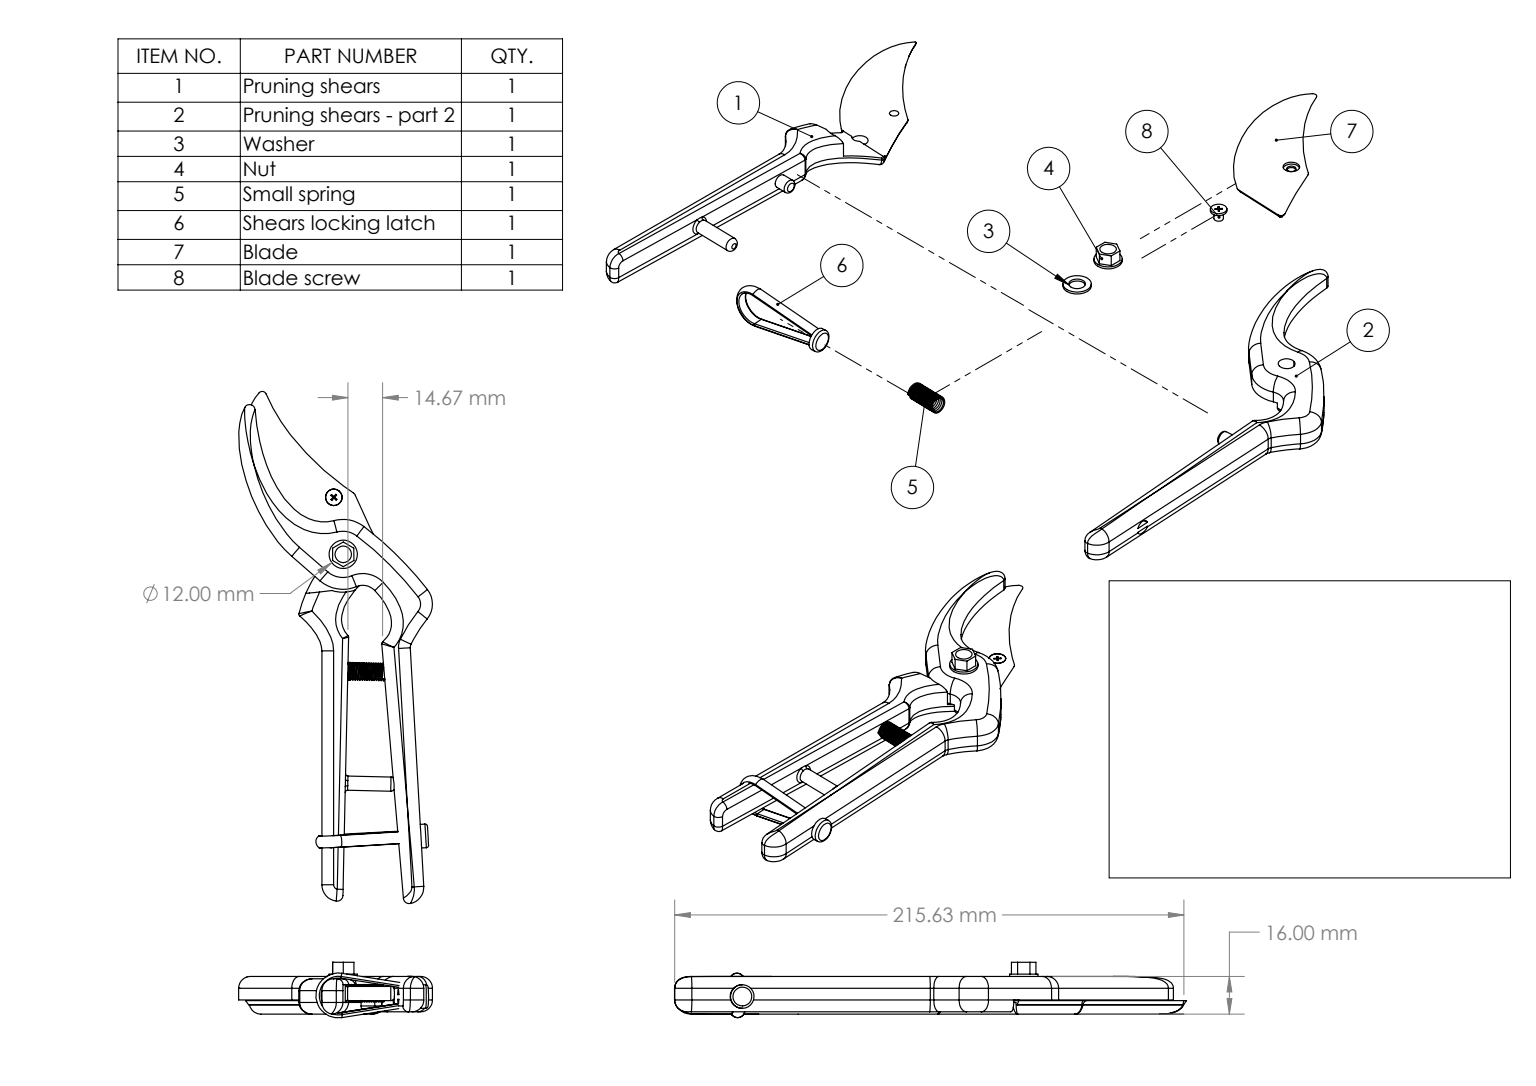
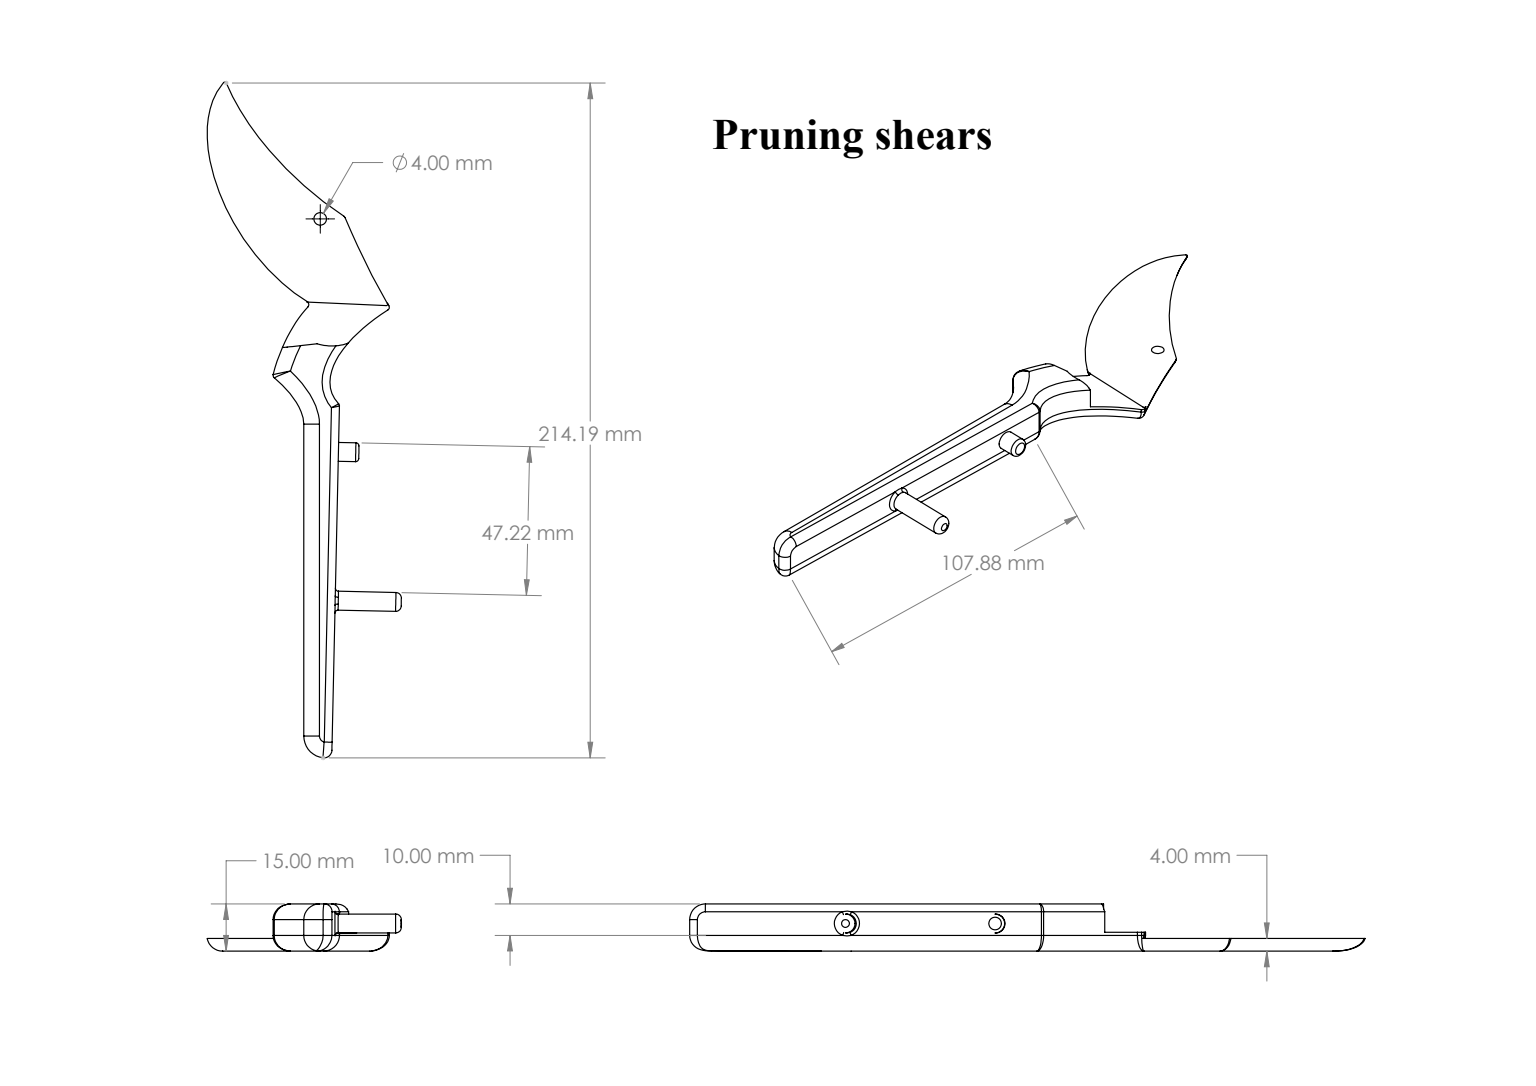
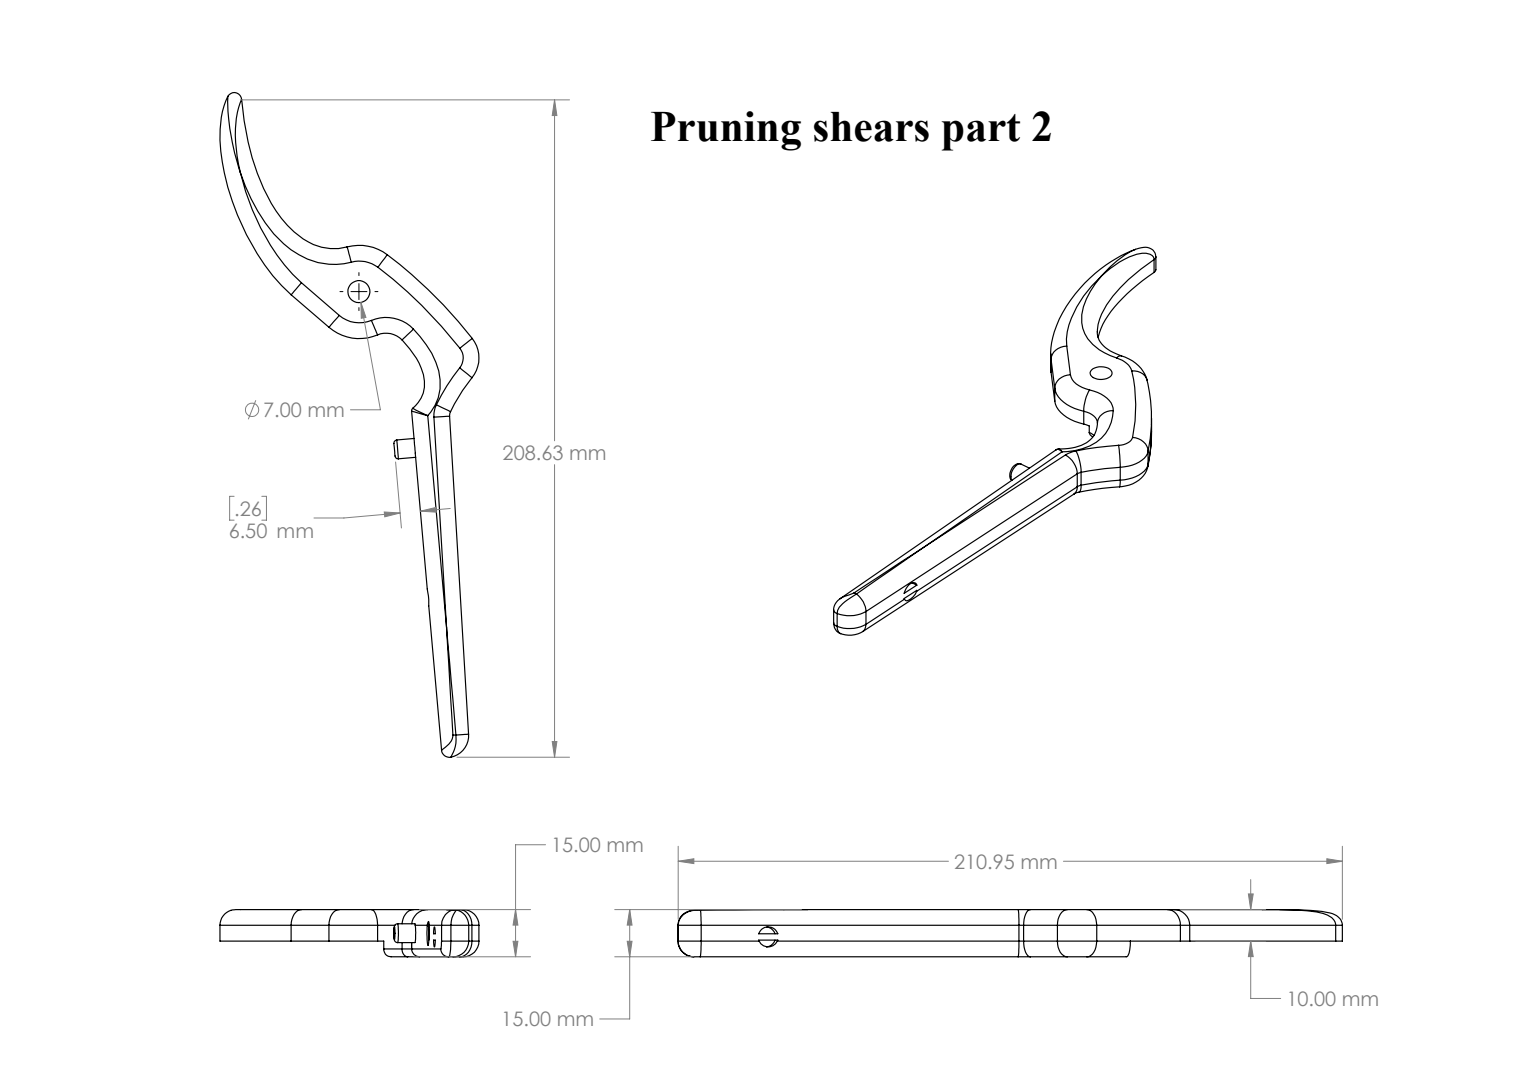
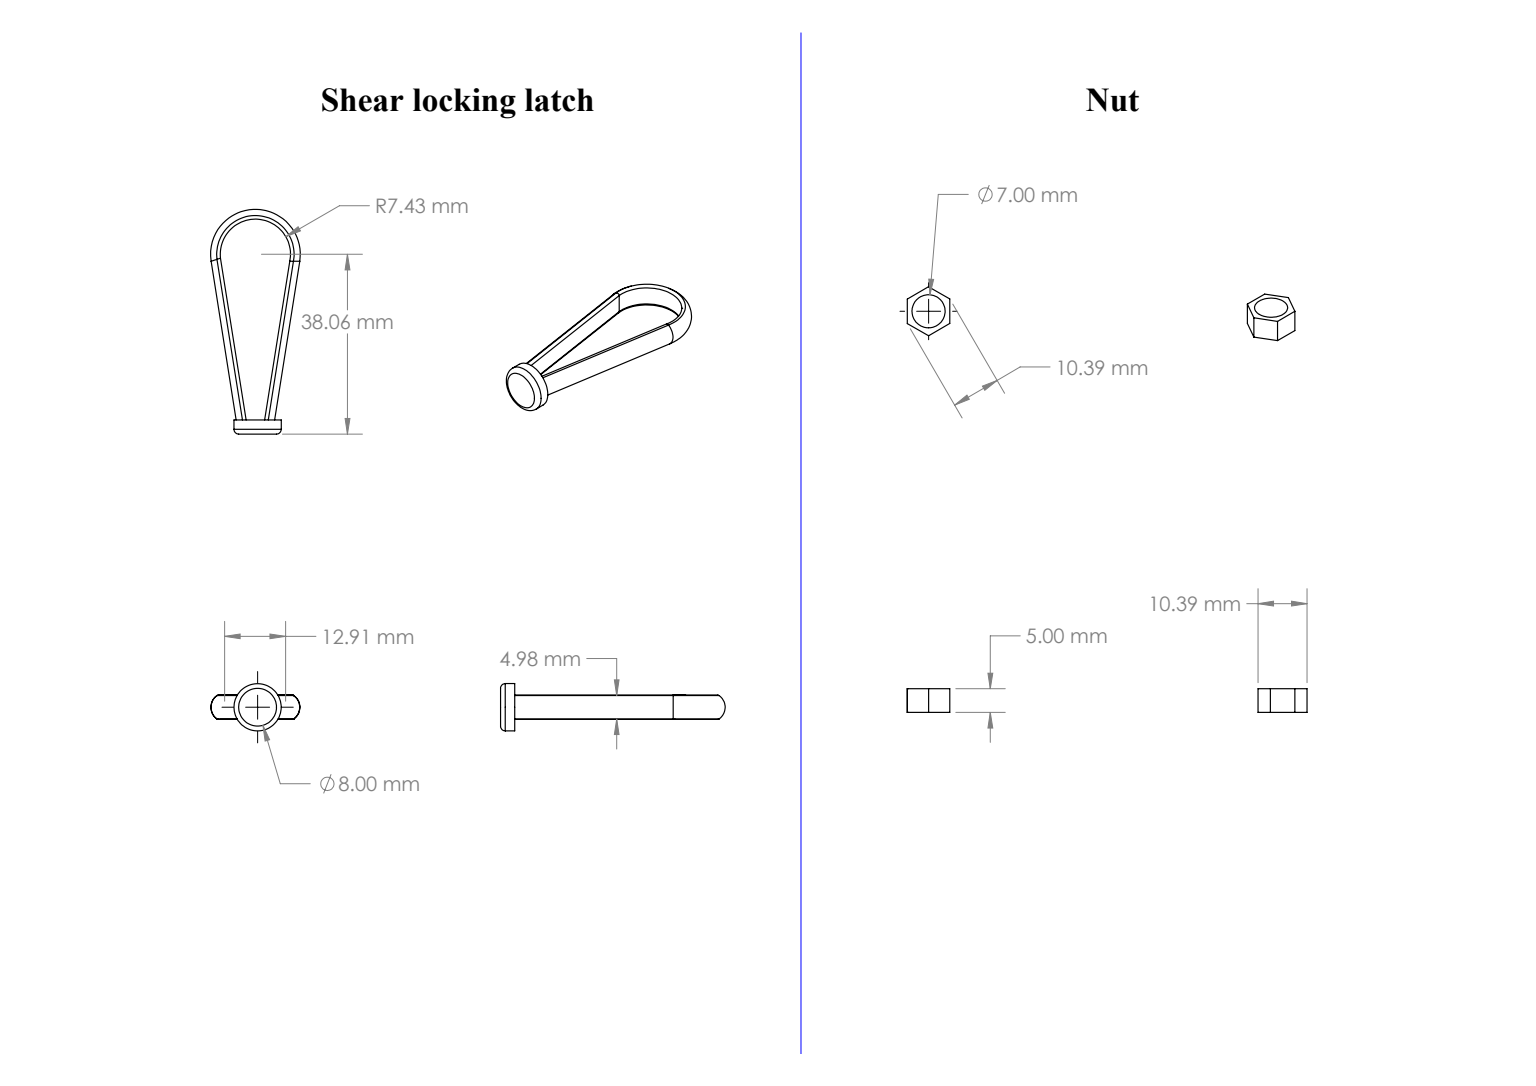
ISO-10303-21;
HEADER;
FILE_DESCRIPTION (('STEP AP203'),
    '1' );
FILE_NAME ('MAS-153',
    '2026-10-08T11:28:20',
    ( '' ),
    ( '' ),
    'SwSTEP 2.0',
    'SolidWorks 2024',
    '' );
FILE_SCHEMA (( 'AUTOMOTIVE_DESIGN' ));
ENDSEC;

DATA;
#1 = B_SPLINE_CURVE_WITH_KNOTS ( 'NONE', 3,
 ( #11082, #3985, #4982, #9929, #8605, #7599 ),
 .UNSPECIFIED., .F., .F.,
 ( 4, 2, 4 ),
 ( 0.000000000000000000, 0.0003771276215161150453, 0.0007542552430322300907 ),
 .UNSPECIFIED. ) ;
#2 = DIRECTION ( 'NONE',  ( 0.000000000000000000, 0.000000000000000000, -1.000000000000000000 ) ) ;
#3 = CARTESIAN_POINT ( 'NONE',  ( 3.749999999999999112, 3.187500000000000444, -5.053300858899108405 ) ) ;
#4 = DIRECTION ( 'NONE',  ( -0.9961255586397056438, 0.000000000000000000, 0.08794243244722428632 ) ) ;
#5 = CARTESIAN_POINT ( 'NONE',  ( -4.239466046644367658, 10.19338654090241114, -48.02051031032586081 ) ) ;
#6 = CARTESIAN_POINT ( 'NONE',  ( 8.895558325401111688, 6.000000000000000000, -141.4560052469132643 ) ) ;
#7 = CC_DESIGN_SECURITY_CLASSIFICATION ( #7654, ( #15322 ) ) ;
#8 = DIRECTION ( 'NONE',  ( 0.003262051938530752433, 0.000000000000000000, 0.9999946794944213346 ) ) ;
#9 = CARTESIAN_POINT ( 'NONE',  ( 3.249999999999999556, 12.75000000000000178, -3.500000000000000000 ) ) ;
#10 =( BOUNDED_SURFACE ( )  B_SPLINE_SURFACE ( 3, 2, ( 
 ( #2250, #5719, #10439 ),
 ( #12764, #3401, #13776 ),
 ( #9122, #8110, #5419 ),
 ( #12528, #2173, #793 ),
 ( #9278, #3171, #9054 ),
 ( #6877, #11445, #7884 ),
 ( #5641, #7962, #13852 ),
 ( #1011, #6953, #14952 ),
 ( #3250, #868, #2099 ),
 ( #10357, #4569, #1944 ),
 ( #15098, #11671, #12608 ),
 ( #4272, #6806, #14003 ),
 ( #12683, #8975, #11522 ),
 ( #3329, #938, #6657 ),
 ( #8038, #13706, #12837 ),
 ( #11370, #3105, #7816 ),
 ( #5571, #9201, #4347 ),
 ( #2023, #6733, #10286 ) ),
 .UNSPECIFIED., .F., .F., .F. ) 
 B_SPLINE_SURFACE_WITH_KNOTS ( ( 4, 2, 2, 2, 2, 2, 2, 2, 4 ),
 ( 3, 3 ),
 ( 0.06508395618386217385, 0.06791873945841907234, 0.07075352273297597083, 0.07217091437025441314, 0.07358830600753285545, 0.07642308928208975394, 0.07925787255664665243, 0.08209265583120353704, 0.08776222238031733403 ),
 ( 0.000000000000000000, 1.000000000000000000 ),
 .UNSPECIFIED. ) 
 GEOMETRIC_REPRESENTATION_ITEM ( )  RATIONAL_B_SPLINE_SURFACE ( (
 ( 1.000000000000000000, 0.7071067811865475727, 1.000000000000000000),
 ( 1.000000000000000000, 0.7071067811865475727, 1.000000000000000000),
 ( 1.000000000000000000, 0.7071067811865475727, 1.000000000000000000),
 ( 1.000000000000000000, 0.7071067811865475727, 1.000000000000000000),
 ( 1.000000000000000000, 0.7071067811865471286, 1.000000000000000000),
 ( 1.000000000000000000, 0.7071067811865471286, 1.000000000000000000),
 ( 1.000000000000000000, 0.7071067811865475727, 1.000000000000000000),
 ( 1.000000000000000000, 0.7071067811865475727, 1.000000000000000000),
 ( 1.000000000000000000, 0.7071067811865475727, 1.000000000000000000),
 ( 1.000000000000000000, 0.7071067811865475727, 1.000000000000000000),
 ( 1.000000000000000000, 0.7071067811865475727, 1.000000000000000000),
 ( 1.000000000000000000, 0.7071067811865475727, 1.000000000000000000),
 ( 1.000000000000000000, 0.7071067811865475727, 1.000000000000000000),
 ( 1.000000000000000000, 0.7071067811865475727, 1.000000000000000000),
 ( 1.000000000000000000, 0.7071067811865475727, 1.000000000000000000),
 ( 1.000000000000000000, 0.7071067811865475727, 1.000000000000000000),
 ( 1.000000000000000000, 0.7071067811865474617, 1.000000000000000000),
 ( 1.000000000000000000, 0.7071067811865474617, 1.000000000000000000) ) ) 
 REPRESENTATION_ITEM ( '' )  SURFACE ( )  );
#11 = AXIS2_PLACEMENT_3D ( 'NONE', #1949, #8982, #6882 ) ;
#12 = CARTESIAN_POINT ( 'NONE',  ( -25.82983890416511841, 9.999999999999998224, -142.4527639562402328 ) ) ;
#13 = CARTESIAN_POINT ( 'NONE',  ( -65.21690963830255328, 14.66435712545321657, -194.0246706955119009 ) ) ;
#14 = CIRCLE ( 'NONE', #8648, 3.500000000000003109 ) ;
#15 = ORIENTED_EDGE ( 'NONE', *, *, #9512, .T. ) ;
#16 = VERTEX_POINT ( 'NONE', #5138 ) ;
#17 = CARTESIAN_POINT ( 'NONE',  ( -6.279162092933343153, 2.500000000000000444, -108.6370948588273535 ) ) ;
#18 = CARTESIAN_POINT ( 'NONE',  ( 11.02991327057161008, 4.000000000000000000, -167.7534593579462125 ) ) ;
#19 = CARTESIAN_POINT ( 'NONE',  ( -3.750000000000000000, 6.250000000000000000, -3.499999999999999112 ) ) ;
#20 = CARTESIAN_POINT ( 'NONE',  ( 3.749999999999999556, 3.250000000000000000, -3.500000000000000444 ) ) ;
#21 = CARTESIAN_POINT ( 'NONE',  ( 1.114947364559086829, 5.000000000000000888, -139.4079432275550232 ) ) ;
#22 = ORIENTED_EDGE ( 'NONE', *, *, #13407, .T. ) ;
#23 = CARTESIAN_POINT ( 'NONE',  ( -6.510167201457561781, 0.4374612817596250647, -117.0692195733290504 ) ) ;
#24 = CARTESIAN_POINT ( 'NONE',  ( -2.298097038856279362, 0.8750000000000000000, -5.798097038856278473 ) ) ;
#25 = AXIS2_PLACEMENT_3D ( 'NONE', #11533, #14885, #11235 ) ;
#26 = CIRCLE ( 'NONE', #8661, 3.250000000000003553 ) ;
#27 = CARTESIAN_POINT ( 'NONE',  ( -46.17421409260412446, 15.00000000000000000, -147.1483150044805939 ) ) ;
#28 = CIRCLE ( 'NONE', #12604, 8.192786906463668473 ) ;
#29 = CARTESIAN_POINT ( 'NONE',  ( 14.17870013830592235, 8.673617379884035472E-16, -133.6038822290509813 ) ) ;
#30 = DIRECTION ( 'NONE',  ( 1.000000000000000000, 0.000000000000000000, 0.000000000000000000 ) ) ;
#31 = CARTESIAN_POINT ( 'NONE',  ( 0.000000000000000000, 3.000000000000000000, -0.2500000000000002220 ) ) ;
#32 = COORDINATED_UNIVERSAL_TIME_OFFSET ( 0, 0, .AHEAD. ) ;
#33 = CARTESIAN_POINT ( 'NONE',  ( 17.45707370880436216, 8.749999999999998224, -89.70141063960701899 ) ) ;
#34 = CARTESIAN_POINT ( 'NONE',  ( 12.21230042249527514, -8.519112334771948619E-13, -124.0782217032746217 ) ) ;
#35 = ORIENTED_EDGE ( 'NONE', *, *, #13499, .F. ) ;
#36 = CARTESIAN_POINT ( 'NONE',  ( -8.661991262811106651, 15.00000000000000000, -130.6821289911104316 ) ) ;
#37 = CARTESIAN_POINT ( 'NONE',  ( -3.249999999999999556, 14.18750000000000000, -2.153805922287440833 ) ) ;
#38 = AXIS2_PLACEMENT_3D ( 'NONE', #940, #8979, #1799 ) ;
#39 = ORIENTED_EDGE ( 'NONE', *, *, #8561, .F. ) ;
#40 = VERTEX_POINT ( 'NONE', #4981 ) ;
#41 = DIRECTION ( 'NONE',  ( -0.000000000000000000, -1.000000000000000000, -0.000000000000000000 ) ) ;
#42 = CARTESIAN_POINT ( 'NONE',  ( 1.553300858899105963, 4.062500000000001776, -7.250000000000000888 ) ) ;
#43 = CARTESIAN_POINT ( 'NONE',  ( -1.346194077712559167, 5.937500000000002665, -6.749999999999999112 ) ) ;
#44 = ORIENTED_EDGE ( 'NONE', *, *, #4143, .F. ) ;
#45 = EDGE_CURVE ( 'NONE', #5739, #9776, #9697, .T. ) ;
#46 = CARTESIAN_POINT ( 'NONE',  ( 4.515869450399739193, 15.00000000000000000, -104.3391973869742060 ) ) ;
#47 = CARTESIAN_POINT ( 'NONE',  ( 1.346194077712558057, 4.562500000000000888, -6.750000000000000000 ) ) ;
#48 = VECTOR ( 'NONE', #1448, 1000.000000000000114 ) ;
#49 = DIRECTION ( 'NONE',  ( -0.002879925520664897674, 0.000000000000000000, -0.9999958530058988826 ) ) ;
#50 = DIRECTION ( 'NONE',  ( 0.000000000000000000, 0.000000000000000000, 1.000000000000000000 ) ) ;
#51 = CARTESIAN_POINT ( 'NONE',  ( -9.030574454602202650, -2.490287375297125294, -34.97919997656153157 ) ) ;
#52 = PERSON_AND_ORGANIZATION ( #3176, #3020 ) ;
#53 = CARTESIAN_POINT ( 'NONE',  ( -48.96897228669091362, 15.00000000000000178, -150.1829960677724500 ) ) ;
#54 = ORIENTED_EDGE ( 'NONE', *, *, #7438, .F. ) ;
#55 =( GEOMETRIC_REPRESENTATION_CONTEXT ( 3 ) GLOBAL_UNCERTAINTY_ASSIGNED_CONTEXT ( ( #2945 ) ) GLOBAL_UNIT_ASSIGNED_CONTEXT ( ( #13919, #7590, #5627 ) ) REPRESENTATION_CONTEXT ( 'NONE', 'WORKASPACE' ) );
#56 = EDGE_CURVE ( 'NONE', #9845, #1534, #14253, .T. ) ;
#57 = DIRECTION ( 'NONE',  ( 0.08794243244723005948, 0.000000000000000000, 0.9961255586397049777 ) ) ;
#58 = ADVANCED_FACE ( 'NONE', ( #12392 ), #3118, .T. ) ;
#59 = CARTESIAN_POINT ( 'NONE',  ( 2.651650429449553314, 14.37500000000000000, -0.8483495705504476847 ) ) ;
#60 = FACE_OUTER_BOUND ( 'NONE', #10831, .T. ) ;
#61 = CARTESIAN_POINT ( 'NONE',  ( -67.60837051205176351, 11.42435839016798838, -204.0214325388246266 ) ) ;
#62 = CARTESIAN_POINT ( 'NONE',  ( 0.5457951471881908878, 3.606183382230925272, -138.3638248956704047 ) ) ;
#63 = CARTESIAN_POINT ( 'NONE',  ( -3.249999999999999556, 3.750000000000000444, -3.500000000000000000 ) ) ;
#64 = CARTESIAN_POINT ( 'NONE',  ( 9.455311519598982528, 14.93740492236557138, -106.0041704794325454 ) ) ;
#65 = APPROVAL_STATUS ( 'not_yet_approved' ) ;
#66 = CARTESIAN_POINT ( 'NONE',  ( -29.69515346086419427, 5.000000000000000888, -156.7390981038714983 ) ) ;
#67 = CARTESIAN_POINT ( 'NONE',  ( -17.09940774937029317, 0.4261086865563343262, -130.4730999849509203 ) ) ;
#68 = ORIENTED_EDGE ( 'NONE', *, *, #7323, .F. ) ;
#69 = CARTESIAN_POINT ( 'NONE',  ( 5.522929128040925839, 0.1436561706274334937, 1.641076506811401270 ) ) ;
#70 = CARTESIAN_POINT ( 'NONE',  ( -3.249999999999999556, 1.250000000000000000, -3.499999999999999556 ) ) ;
#71 = AXIS2_PLACEMENT_3D ( 'NONE', #14775, #7400, #12125 ) ;
#72 = CARTESIAN_POINT ( 'NONE',  ( -63.46632602869123474, 15.00000000000000000, -179.6775508400713477 ) ) ;
#73 = CARTESIAN_POINT ( 'NONE',  ( 2.298097038856278029, 7.125000000000000888, -5.798097038856279362 ) ) ;
#74 = ORIENTED_EDGE ( 'NONE', *, *, #3541, .T. ) ;
#75 = CARTESIAN_POINT ( 'NONE',  ( -5.117107008692297399, 9.999999999999998224, -113.5915292474705893 ) ) ;
#76 = EDGE_CURVE ( 'NONE', #2801, #15277, #3494, .T. ) ;
#77 = CARTESIAN_POINT ( 'NONE',  ( 21.59580923397518859, 6.000000000000000000, -133.6052420832058374 ) ) ;
#78 = CARTESIAN_POINT ( 'NONE',  ( 9.096999351293019842, 14.99999999999896438, -106.0212576677412812 ) ) ;
#79 = CARTESIAN_POINT ( 'NONE',  ( 2.298097038856279362, 1.875000000000000000, -1.201902961143720860 ) ) ;
#80 = CARTESIAN_POINT ( 'NONE',  ( -1.553300858899107073, 1.937500000000000222, -7.249999999999999112 ) ) ;
#81 = APPLICATION_CONTEXT ( 'configuration controlled 3d designs of mechanical parts and assemblies' ) ;
#82 = CARTESIAN_POINT ( 'NONE',  ( -3.750000000000000000, 7.312500000000000000, -5.053300858899105741 ) ) ;
#83 = CARTESIAN_POINT ( 'NONE',  ( -0.2962205294200081496, 8.673617379884033500E-16, -113.2751335308100096 ) ) ;
#84 = CARTESIAN_POINT ( 'NONE',  ( 3.749999999999999556, 4.250000000000000000, -3.500000000000000444 ) ) ;
#85 = CIRCLE ( 'NONE', #9462, 0.4999999999999865663 ) ;
#86 = CARTESIAN_POINT ( 'NONE',  ( 1.062740323768540662, 12.59030360039310636, 5.094619354848065385 ) ) ;
#87 = DIRECTION ( 'NONE',  ( 0.000000000000000000, 0.000000000000000000, -1.000000000000000000 ) ) ;
#88 = CARTESIAN_POINT ( 'NONE',  ( -0.3675725891509493137, 0.000000000000000000, -0.3389548520155291622 ) ) ;
#89 = LINE ( 'NONE', #4800, #3326 ) ;
#90 = CARTESIAN_POINT ( 'NONE',  ( 1.346194077712560944, 10.93750000000000000, -0.2500000000000010547 ) ) ;
#91 = CARTESIAN_POINT ( 'NONE',  ( 8.807773658247754156, 15.00000000000000000, -105.8689255569352667 ) ) ;
#92 = CARTESIAN_POINT ( 'NONE',  ( -63.21422130130005712, 10.26968228116884596, -203.6040552426024988 ) ) ;
#93 = ORIENTED_EDGE ( 'NONE', *, *, #14365, .F. ) ;
#94 = ORIENTED_EDGE ( 'NONE', *, *, #15196, .T. ) ;
#95 = CARTESIAN_POINT ( 'NONE',  ( -4.723546506723169003, 4.336808689942017736E-16, -121.1708306026675501 ) ) ;
#96 = CARTESIAN_POINT ( 'NONE',  ( 10.93680211553660619, 8.749999999999998224, -88.84347220940026091 ) ) ;
#97 = CARTESIAN_POINT ( 'NONE',  ( 3.749999999999998668, 4.687500000000000888, -5.053300858899107517 ) ) ;
#98 = AXIS2_PLACEMENT_3D ( 'NONE', #12343, #1762, #3856 ) ;
#99 = CARTESIAN_POINT ( 'NONE',  ( -3.750000000000000000, 5.812500000000000888, -5.053300858899105741 ) ) ;
#100 = AXIS2_PLACEMENT_3D ( 'NONE', #7008, #14909, #675 ) ;
#101 = DIRECTION ( 'NONE',  ( -0.02181900108494732801, 0.000000000000000000, 0.9997619372588931741 ) ) ;
#102 = ORIENTED_EDGE ( 'NONE', *, *, #10097, .F. ) ;
#103 = CARTESIAN_POINT ( 'NONE',  ( 3.249999999999998224, 3.187500000000000444, -4.846194077712561388 ) ) ;
#104 = CARTESIAN_POINT ( 'NONE',  ( -54.45540687895485377, 9.999999999999998224, -149.0501727870129685 ) ) ;
#105 = DIRECTION ( 'NONE',  ( 0.000000000000000000, 1.000000000000000000, 0.000000000000000000 ) ) ;
#106 = CARTESIAN_POINT ( 'NONE',  ( -2.298097038856278918, 2.375000000000000000, -5.798097038856277585 ) ) ;
#107 = AXIS2_PLACEMENT_3D ( 'NONE', #15128, #4596, #14185 ) ;
#108 = PERSON_AND_ORGANIZATION_ROLE ( 'classification_officer' ) ;
#109 = CARTESIAN_POINT ( 'NONE',  ( 10.14688567188825274, 12.49999999999999822, -108.1982192590441088 ) ) ;
#110 = CARTESIAN_POINT ( 'NONE',  ( 16.81337476685454391, 5.000000000000000888, -129.2521154345601246 ) ) ;
#111 = ORIENTED_EDGE ( 'NONE', *, *, #10885, .F. ) ;
#112 = CARTESIAN_POINT ( 'NONE',  ( -0.5447792503669787179, 14.99999999999999467, -117.0548960884185732 ) ) ;
#113 = CARTESIAN_POINT ( 'NONE',  ( 1.346194077712560944, 14.93750000000000178, -0.2500000000000011102 ) ) ;
#114 = VERTEX_POINT ( 'NONE', #6524 ) ;
#115 = EDGE_LOOP ( 'NONE', ( #2577, #6448, #3644, #14462 ) ) ;
#116 = DIRECTION ( 'NONE',  ( -0.000000000000000000, -1.000000000000000000, -0.000000000000000000 ) ) ;
#117 = CARTESIAN_POINT ( 'NONE',  ( -4.592425496802573972E-16, 5.000000000000000000, -7.250000000000000000 ) ) ;
#118 = CARTESIAN_POINT ( 'NONE',  ( -1.346194077712558945, 10.56249999999999822, -0.2500000000000002220 ) ) ;
#119 = VERTEX_POINT ( 'NONE', #1731 ) ;
#120 = CARTESIAN_POINT ( 'NONE',  ( -1.334601435215557519, 9.999999999999998224, -105.6792246796216403 ) ) ;
#121 = CIRCLE ( 'NONE', #7519, 4.999999999999995559 ) ;
#122 = CARTESIAN_POINT ( 'NONE',  ( 1.346194077712558057, 3.562500000000000444, -6.750000000000000000 ) ) ;
#123 = CARTESIAN_POINT ( 'NONE',  ( -7.332173456847238313, 0.07668794466513038921, -104.2603615701598869 ) ) ;
#124 = CARTESIAN_POINT ( 'NONE',  ( -62.71861979978048396, 10.00000000000000000, -198.6004802465432135 ) ) ;
#125 = AXIS2_PLACEMENT_3D ( 'NONE', #9268, #6866, #11579 ) ;
#126 = SHAPE_DEFINITION_REPRESENTATION ( #5707, #10790 ) ;
#127 = CARTESIAN_POINT ( 'NONE',  ( -52.99646050385619844, 15.00000000000000000, -155.6021463114098253 ) ) ;
#128 = ORIENTED_EDGE ( 'NONE', *, *, #6104, .F. ) ;
#129 = CARTESIAN_POINT ( 'NONE',  ( -3.249999999999999556, 9.187500000000000000, -2.153805922287440833 ) ) ;
#130 = CARTESIAN_POINT ( 'NONE',  ( -4.234402844927150689, 15.00000000000000000, -117.4888040839639558 ) ) ;
#131 = CARTESIAN_POINT ( 'NONE',  ( -4.592425496802573972E-16, 14.00000000000000000, -7.250000000000000000 ) ) ;
#132 = CARTESIAN_POINT ( 'NONE',  ( 0.000000000000000000, 0.000000000000000000, -2.000000000000000000 ) ) ;
#133 = B_SPLINE_CURVE_WITH_KNOTS ( 'NONE', 3,
 ( #5793, #4490, #6875, #8036, #2247, #9119, #866, #3327, #10513, #12761, #13773, #3478, #11520, #10215, #15248, #4639, #8187, #5717, #11590, #14950, #12912, #2325, #9052, #7024 ),
 .UNSPECIFIED., .F., .F.,
 ( 4, 2, 2, 2, 2, 2, 2, 2, 2, 2, 2, 4 ),
 ( 0.001027084968682773474, 0.001754664737541044694, 0.002482244506399315480, 0.003937404044115912563, 0.004664983812974211538, 0.005392563581832510514, 0.006847723119549108464, 0.009758042194982304365, 0.01121320173269890232, 0.01194078150155724292, 0.01230457138598641496, 0.01266836127041558527 ),
 .UNSPECIFIED. ) ;
#134 = CARTESIAN_POINT ( 'NONE',  ( -63.23239576043733479, 10.46432717375524213, -203.5646039687676705 ) ) ;
#135 = CARTESIAN_POINT ( 'NONE',  ( 0.5065669489467078401, 5.000000000003537615, 5.737893198614711032 ) ) ;
#136 = CARTESIAN_POINT ( 'NONE',  ( 1.346194077712561166, 4.437500000000001776, -0.2500000000000011102 ) ) ;
#137 = ADVANCED_FACE ( 'NONE', ( #11160 ), #2010, .F. ) ;
#138 = CARTESIAN_POINT ( 'NONE',  ( 9.910078351765200466, 14.75237657882121667, -106.1010689402279468 ) ) ;
#139 = PERSON_AND_ORGANIZATION ( #3176, #3020 ) ;
#140 = EDGE_CURVE ( 'NONE', #13676, #587, #14399, .T. ) ;
#141 = CARTESIAN_POINT ( 'NONE',  ( 1.855481649321436777, 15.00000000000000000, -35.83830032691820122 ) ) ;
#142 = CARTESIAN_POINT ( 'NONE',  ( 0.000000000000000000, 5.000000000000000000, -3.500000000000000000 ) ) ;
#143 = EDGE_LOOP ( 'NONE', ( #10004, #6723, #11790, #8217 ) ) ;
#144 = CARTESIAN_POINT ( 'NONE',  ( 5.475582110871519248, 2.099780042704602945, 4.221432182364227792 ) ) ;
#145 = CARTESIAN_POINT ( 'NONE',  ( 2.298097038856279362, 1.875000000000000000, -1.201902961143720860 ) ) ;
#146 = CARTESIAN_POINT ( 'NONE',  ( -9.240119717473294969, 2.324218168632100845, -104.6630069163585972 ) ) ;
#147 = CARTESIAN_POINT ( 'NONE',  ( 3.249999999999999556, 14.75000000000000178, -3.500000000000000000 ) ) ;
#148 = CARTESIAN_POINT ( 'NONE',  ( -1.346194077712559167, 5.937500000000002665, -6.749999999999999112 ) ) ;
#149 = ORIENTED_EDGE ( 'NONE', *, *, #4890, .T. ) ;
#150 = CARTESIAN_POINT ( 'NONE',  ( -5.893421222731322295, 9.999999999999998224, -117.5694263798337005 ) ) ;
#151 = DIRECTION ( 'NONE',  ( 0.000000000000000000, 1.000000000000000000, 0.000000000000000000 ) ) ;
#152 = CARTESIAN_POINT ( 'NONE',  ( 1.818681402055029483, 15.00000000000000000, -137.3269588978979243 ) ) ;
#153 = CC_DESIGN_DATE_AND_TIME_ASSIGNMENT ( #8465, #10947, ( #9370 ) ) ;
#154 = CARTESIAN_POINT ( 'NONE',  ( -2.298097038856278918, 0.3750000000000000000, -5.798097038856277585 ) ) ;
#155 = CARTESIAN_POINT ( 'NONE',  ( 2.651650429449552870, 1.124999999999999778, -6.151650429449553314 ) ) ;
#156 = CARTESIAN_POINT ( 'NONE',  ( -2.651650429449552870, 4.125000000000000000, -0.8483495705504462414 ) ) ;
#157 = CARTESIAN_POINT ( 'NONE',  ( -5.309262520577839872, 13.36526483154179523, -125.0911079416483176 ) ) ;
#158 = CARTESIAN_POINT ( 'NONE',  ( 2.651650429449552870, 8.125000000000000000, -6.151650429449555091 ) ) ;
#159 = CARTESIAN_POINT ( 'NONE',  ( 0.9143209798285035772, 12.53633980243307100, 2.514521240264253166 ) ) ;
#160 = DIRECTION ( 'NONE',  ( 0.000000000000000000, -0.000000000000000000, 1.000000000000000000 ) ) ;
#161 = EDGE_CURVE ( 'NONE', #6131, #12717, #6840, .T. ) ;
#162 = EDGE_CURVE ( 'NONE', #10108, #12142, #11036, .T. ) ;
#163 = DIRECTION ( 'NONE',  ( -0.000000000000000000, 1.000000000000000000, -0.000000000000000000 ) ) ;
#164 = EDGE_CURVE ( 'NONE', #10316, #6640, #6443, .T. ) ;
#165 = FACE_OUTER_BOUND ( 'NONE', #967, .T. ) ;
#166 = CARTESIAN_POINT ( 'NONE',  ( 0.000000000000000000, 14.00000000000000000, -0.2500000000000002220 ) ) ;
#167 = CARTESIAN_POINT ( 'NONE',  ( 8.617011912565523346, 3.196949058014985745, 2.666643044219553893 ) ) ;
#168 = CARTESIAN_POINT ( 'NONE',  ( -64.38825976928389139, 13.56900998018364213, -200.2675612624753398 ) ) ;
#169 = ORIENTED_EDGE ( 'NONE', *, *, #3673, .F. ) ;
#170 = CARTESIAN_POINT ( 'NONE',  ( -3.749999999999999556, 8.750000000000000000, -3.499999999999999112 ) ) ;
#171 = EDGE_LOOP ( 'NONE', ( #12222, #10076, #8001, #12391 ) ) ;
#172 = CARTESIAN_POINT ( 'NONE',  ( -6.790118584858316986, 2.500000000000000444, -107.8021323224912464 ) ) ;
#173 = CARTESIAN_POINT ( 'NONE',  ( -10.72138378296756756, -1.921202954650397476, -40.62330995231929620 ) ) ;
#174 = CARTESIAN_POINT ( 'NONE',  ( 1.553300858899108849, 9.937499999999998224, 0.2499999999999993616 ) ) ;
#175 = CARTESIAN_POINT ( 'NONE',  ( -3.749999999999999556, 5.750000000000000000, -3.499999999999999112 ) ) ;
#176 = DIRECTION ( 'NONE',  ( -0.9997619372588932851, -0.000000000000000000, -0.02181900108494707474 ) ) ;
#177 = ORIENTED_EDGE ( 'NONE', *, *, #10342, .F. ) ;
#178 = CARTESIAN_POINT ( 'NONE',  ( -2.298097038856278029, 2.625000000000000000, -1.201902961143720638 ) ) ;
#179 = CARTESIAN_POINT ( 'NONE',  ( -69.61556017177876754, 9.999999999999998224, -198.3353672694111083 ) ) ;
#180 = CARTESIAN_POINT ( 'NONE',  ( 19.46764420669212470, 5.416677968589100837E-32, -137.9817351395554681 ) ) ;
#181 = CARTESIAN_POINT ( 'NONE',  ( 2.298097038856279362, 6.875000000000000000, -1.201902961143720860 ) ) ;
#182 = CARTESIAN_POINT ( 'NONE',  ( -1.794496370643203553, 15.00000000000000711, -123.9659188807642920 ) ) ;
#183 = APPROVAL_ROLE ( '' ) ;
#184 = CARTESIAN_POINT ( 'NONE',  ( -4.891470111510197505, 6.071532165918824830E-15, -115.0631877436127581 ) ) ;
#185 = CARTESIAN_POINT ( 'NONE',  ( 20.93263444585494781, -4.267469463954428261E-13, -132.7914611339567159 ) ) ;
#186 = CC_DESIGN_DATE_AND_TIME_ASSIGNMENT ( #10259, #7786, ( #13819 ) ) ;
#187 = ORIENTED_EDGE ( 'NONE', *, *, #1290, .T. ) ;
#188 = CARTESIAN_POINT ( 'NONE',  ( -1.260792021077014269, 15.00000000000000178, -107.5178971017766258 ) ) ;
#189 = CARTESIAN_POINT ( 'NONE',  ( -3.980102097228897245E-16, 14.50000000000000000, -6.749999999999999112 ) ) ;
#190 = ORIENTED_EDGE ( 'NONE', *, *, #14252, .F. ) ;
#191 = VERTEX_POINT ( 'NONE', #10233 ) ;
#192 = CARTESIAN_POINT ( 'NONE',  ( 22.32840821305085655, 0.1344125794277489794, -138.8040290914306922 ) ) ;
#193 = CARTESIAN_POINT ( 'NONE',  ( 2.651650429449552870, 7.125000000000000888, -6.151650429449555091 ) ) ;
#194 = CARTESIAN_POINT ( 'NONE',  ( -2.298097038856279362, 8.874999999999996447, -5.798097038856278473 ) ) ;
#195 = ORIENTED_EDGE ( 'NONE', *, *, #5701, .F. ) ;
#196 = CARTESIAN_POINT ( 'NONE',  ( 6.130233522805849766, 11.30590447954031497, 5.118507051967887911 ) ) ;
#197 = CARTESIAN_POINT ( 'NONE',  ( -3.249999999999999556, 5.187500000000001776, -2.153805922287440833 ) ) ;
#198 = CARTESIAN_POINT ( 'NONE',  ( -9.222297982611349809, 2.161611222164042001, -104.6591137165734864 ) ) ;
#199 = CARTESIAN_POINT ( 'NONE',  ( -33.91109452337774854, 10.00000000000000178, -156.1716796081737471 ) ) ;
#200 = CARTESIAN_POINT ( 'NONE',  ( -45.43402158771803556, 15.00000000000000355, -154.4665057826428267 ) ) ;
#201 = APPROVAL_ROLE ( '' ) ;
#202 = CARTESIAN_POINT ( 'NONE',  ( -62.77354874813351415, 14.99999999999999822, -176.9788886477732035 ) ) ;
#203 = ORIENTED_EDGE ( 'NONE', *, *, #9865, .F. ) ;
#204 = CARTESIAN_POINT ( 'NONE',  ( -3.249999999999999556, 0.3125000000000000555, -4.846194077712557835 ) ) ;
#205 = CARTESIAN_POINT ( 'NONE',  ( -0.9850606648477213678, 15.00000000000000000, -125.5681744140592144 ) ) ;
#206 = CARTESIAN_POINT ( 'NONE',  ( -3.750000000000000000, 12.81250000000000178, -5.053300858899105741 ) ) ;
#207 = CARTESIAN_POINT ( 'NONE',  ( -67.63619164393119831, 12.59430211938552802, -202.7040278164101323 ) ) ;
#208 = DIRECTION ( 'NONE',  ( -0.9997619372588932851, -0.000000000000000000, -0.02181900108494707821 ) ) ;
#209 = CARTESIAN_POINT ( 'NONE',  ( 1.346194077712561166, 3.437500000000000444, -0.2500000000000011102 ) ) ;
#210 = CARTESIAN_POINT ( 'NONE',  ( 9.985685122837379524, 1.585996910455645059, -106.2985558885148833 ) ) ;
#211 = PERSON_AND_ORGANIZATION ( #3176, #3020 ) ;
#212 = CARTESIAN_POINT ( 'NONE',  ( -2.555845825458327170, 14.83119756125146438, -125.3948779398220381 ) ) ;
#213 = CARTESIAN_POINT ( 'NONE',  ( -9.030574454602195544, -2.490287375297125294, -34.97919997656152447 ) ) ;
#214 = ORIENTED_EDGE ( 'NONE', *, *, #4803, .T. ) ;
#215 = CARTESIAN_POINT ( 'NONE',  ( 5.309569511722092905, 0.1704923354856621165, -0.3824473862144103231 ) ) ;
#216 = CARTESIAN_POINT ( 'NONE',  ( -2.298097038856278918, 8.375000000000000000, -5.798097038856277585 ) ) ;
#217 = CARTESIAN_POINT ( 'NONE',  ( -63.86794096056340209, 10.00000000000000000, -165.1728739221729825 ) ) ;
#218 = CARTESIAN_POINT ( 'NONE',  ( 2.298097038856278473, 14.62500000000000000, -5.798097038856279362 ) ) ;
#219 = EDGE_CURVE ( 'NONE', #9239, #1748, #2967, .T. ) ;
#220 = CARTESIAN_POINT ( 'NONE',  ( 0.000000000000000000, 7.500000000000000888, -0.2500000000000002220 ) ) ;
#221 = CARTESIAN_POINT ( 'NONE',  ( -0.5758322980023804494, 15.00000000000000000, -117.2003571699043221 ) ) ;
#222 = DIRECTION ( 'NONE',  ( 0.000000000000000000, 0.000000000000000000, 1.000000000000000000 ) ) ;
#223 = CARTESIAN_POINT ( 'NONE',  ( 6.020998550613693823, 15.00000000000000000, -132.6181299100952629 ) ) ;
#224 = EDGE_CURVE ( 'NONE', #10778, #11957, #683, .T. ) ;
#225 = CARTESIAN_POINT ( 'NONE',  ( 2.298097038856278473, 1.625000000000000222, -5.798097038856279362 ) ) ;
#226 = CARTESIAN_POINT ( 'NONE',  ( -2.651650429449552870, 2.625000000000000000, -0.8483495705504467965 ) ) ;
#227 = CARTESIAN_POINT ( 'NONE',  ( 1.553300858899108849, 4.937500000000000888, 0.2499999999999993616 ) ) ;
#228 = CARTESIAN_POINT ( 'NONE',  ( -4.160651409637847742, 10.31235003438523989, -46.92824181062579214 ) ) ;
#229 = CARTESIAN_POINT ( 'NONE',  ( 1.553300858899105963, 6.062500000000000888, -7.250000000000000888 ) ) ;
#230 = CARTESIAN_POINT ( 'NONE',  ( 1.674841001514616012, 13.54983687837186146, 4.356007712918980701 ) ) ;
#231 = CARTESIAN_POINT ( 'NONE',  ( -3.806000526524415672, 10.67725751578602633, -43.60682525637299989 ) ) ;
#232 =( BOUNDED_SURFACE ( )  B_SPLINE_SURFACE ( 3, 1, ( 
 ( #3931, #529 ),
 ( #12031, #14691 ),
 ( #8632, #9877 ),
 ( #298, #8796 ) ),
 .UNSPECIFIED., .F., .F., .T. ) 
 B_SPLINE_SURFACE_WITH_KNOTS ( ( 4, 4 ),
 ( 2, 2 ),
 ( 0.000000000000000000, 1.000000000000000000 ),
 ( 0.000000000000000000, 1.000000000000000000 ),
 .UNSPECIFIED. ) 
 GEOMETRIC_REPRESENTATION_ITEM ( )  RATIONAL_B_SPLINE_SURFACE ( (
 ( 1.000000000000000000, 1.000000000000000000),
 ( 0.6468719831415908894, 0.6468719831415908894),
 ( 0.6468719831415908894, 0.6468719831415908894),
 ( 1.000000000000000000, 1.000000000000000000) ) ) 
 REPRESENTATION_ITEM ( '' )  SURFACE ( )  );
#233 = FACE_OUTER_BOUND ( 'NONE', #599, .T. ) ;
#234 = CC_DESIGN_DATE_AND_TIME_ASSIGNMENT ( #2614, #2772, ( #2984 ) ) ;
#235 = DIRECTION ( 'NONE',  ( 0.9997619372588932851, -0.000000000000000000, 0.02181900108494707474 ) ) ;
#236 = LINE ( 'NONE', #6346, #3220 ) ;
#237 = CARTESIAN_POINT ( 'NONE',  ( -19.59630400042128784, 8.673617379884035472E-16, -169.8472985358678216 ) ) ;
#238 = CARTESIAN_POINT ( 'NONE',  ( 9.939878312292623974, 5.000000000000000888, -115.2320631035898373 ) ) ;
#239 = CARTESIAN_POINT ( 'NONE',  ( 1.346194077712560944, 8.937500000000001776, -0.2500000000000010547 ) ) ;
#240 = ORIENTED_EDGE ( 'NONE', *, *, #10815, .T. ) ;
#241 = LOCAL_TIME ( 12, 28, 20.00000000000000000, #1669 ) ;
#242 = CARTESIAN_POINT ( 'NONE',  ( -3.750000000000000000, 10.81250000000000000, -5.053300858899105741 ) ) ;
#243 = EDGE_LOOP ( 'NONE', ( #11028, #10928, #1338, #8785, #9085 ) ) ;
#244 = CARTESIAN_POINT ( 'NONE',  ( -4.448900195745486563, 0.000000000000000000, -120.6207097488509703 ) ) ;
#245 = CARTESIAN_POINT ( 'NONE',  ( -9.836272398077410273, -1.921202954650397032, -34.71741284551207229 ) ) ;
#246 = CARTESIAN_POINT ( 'NONE',  ( 2.651650429449553759, 9.875000000000000000, -0.8483495705504471296 ) ) ;
#247 = CARTESIAN_POINT ( 'NONE',  ( 3.749999999999998668, 4.187500000000000888, -5.053300858899108405 ) ) ;
#248 = CIRCLE ( 'NONE', #2460, 11.99999999999995559 ) ;
#249 = CARTESIAN_POINT ( 'NONE',  ( -17.72297831578844196, 1.105884851291182525, -129.7878113374480904 ) ) ;
#250 = ORIENTED_EDGE ( 'NONE', *, *, #1589, .T. ) ;
#251 = CARTESIAN_POINT ( 'NONE',  ( 2.298097038856278029, 5.125000000000000000, -5.798097038856279362 ) ) ;
#252 = ADVANCED_FACE ( 'NONE', ( #14573 ), #14420, .T. ) ;
#253 = CARTESIAN_POINT ( 'NONE',  ( 2.651650429449553759, 10.87500000000000178, -0.8483495705504471296 ) ) ;
#254 = CARTESIAN_POINT ( 'NONE',  ( -69.46795959494568251, 14.99999999999999645, -199.1268727653549320 ) ) ;
#255 = B_SPLINE_CURVE_WITH_KNOTS ( 'NONE', 3,
 ( #476, #7341, #3878, #8660, #12368, #14639, #2797, #7574, #10984, #1631 ),
 .UNSPECIFIED., .F., .F.,
 ( 4, 2, 2, 2, 4 ),
 ( 2.327414349645749169E-05, 0.0008162123097076399297, 0.001609150475918822527, 0.002402088642130005124, 0.003195026808341187505 ),
 .UNSPECIFIED. ) ;
#256 = LOCAL_TIME ( 12, 28, 20.00000000000000000, #2505 ) ;
#257 = CARTESIAN_POINT ( 'NONE',  ( -8.749806588114534378, 5.000000000000000888, -116.1271478199639944 ) ) ;
#258 = CARTESIAN_POINT ( 'NONE',  ( 3.249999999999998668, 8.687500000000000000, -4.846194077712560500 ) ) ;
#259 = AXIS2_PLACEMENT_3D ( 'NONE', #6513, #5353, #11151 ) ;
#260 = CARTESIAN_POINT ( 'NONE',  ( -0.3766621274091715987, 0.2398196381212478467, -0.1347136637304948426 ) ) ;
#261 = CALENDAR_DATE ( 2026, 8, 10 ) ;
#262 = CARTESIAN_POINT ( 'NONE',  ( -3.149239014774738887, 4.336808689942018525E-15, -131.9551168574780320 ) ) ;
#263 = CARTESIAN_POINT ( 'NONE',  ( 21.65409573403057664, 5.000000000000000888, -133.3516700273328581 ) ) ;
#264 = ORIENTED_EDGE ( 'NONE', *, *, #11581, .T. ) ;
#265 = CARTESIAN_POINT ( 'NONE',  ( 10.97171279554003043, 8.773889247172311556, -44.61149169061435060 ) ) ;
#266 = DIRECTION ( 'NONE',  ( -0.08794243244722425856, -0.000000000000000000, -0.9961255586397054218 ) ) ;
#267 = ORIENTED_EDGE ( 'NONE', *, *, #4780, .T. ) ;
#268 = ORIENTED_EDGE ( 'NONE', *, *, #15190, .T. ) ;
#269 = CARTESIAN_POINT ( 'NONE',  ( 26.64344053652503774, 3.212383873964119285, -138.2698333691874382 ) ) ;
#270 = CARTESIAN_POINT ( 'NONE',  ( -3.750000000000000000, 10.68750000000000178, -1.946699141100893149 ) ) ;
#271 = CARTESIAN_POINT ( 'NONE',  ( 1.346194077712558279, 6.062500000000000000, -6.750000000000000888 ) ) ;
#272 = CARTESIAN_POINT ( 'NONE',  ( -3.249999999999999556, 10.75000000000000000, -3.500000000000000000 ) ) ;
#273 = VERTEX_POINT ( 'NONE', #7283 ) ;
#274 = VECTOR ( 'NONE', #10771, 1000.000000000000000 ) ;
#275 = CARTESIAN_POINT ( 'NONE',  ( -11.39745071144076860, 8.673617379884034486E-16, -180.6895918776547774 ) ) ;
#276 = AXIS2_PLACEMENT_3D ( 'NONE', #7500, #13311, #2716 ) ;
#277 = CARTESIAN_POINT ( 'NONE',  ( -2.298097038856278473, 5.125000000000000000, -1.201902961143720416 ) ) ;
#278 = AXIS2_PLACEMENT_3D ( 'NONE', #4367, #11396, #11245 ) ;
#279 = ADVANCED_FACE ( 'NONE', ( #4972 ), #9605, .T. ) ;
#280 = CARTESIAN_POINT ( 'NONE',  ( -8.229629558439073733, 0.4823876599422149414, -104.4461881430476069 ) ) ;
#281 = FACE_OUTER_BOUND ( 'NONE', #1053, .T. ) ;
#282 = DIRECTION ( 'NONE',  ( 0.000000000000000000, 1.000000000000000000, 0.000000000000000000 ) ) ;
#283 = PERSON_AND_ORGANIZATION_ROLE ( 'creator' ) ;
#284 = AXIS2_PLACEMENT_3D ( 'NONE', #14005, #3560, #9280 ) ;
#285 = CARTESIAN_POINT ( 'NONE',  ( -24.73595349569526292, 2.956764506585224606, -208.3499888930396651 ) ) ;
#286 = ORIENTED_EDGE ( 'NONE', *, *, #1844, .F. ) ;
#287 = CARTESIAN_POINT ( 'NONE',  ( 2.298097038856279362, 0.8750000000000000000, -1.201902961143720860 ) ) ;
#288 = CARTESIAN_POINT ( 'NONE',  ( -1.553300858899107295, 11.43750000000000000, -7.250000000000000000 ) ) ;
#289 = LINE ( 'NONE', #1755, #10684 ) ;
#290 = AXIS2_PLACEMENT_3D ( 'NONE', #10491, #9174, #1135 ) ;
#291 = CARTESIAN_POINT ( 'NONE',  ( -2.651650429449552870, 11.62500000000000000, -0.8483495705504467965 ) ) ;
#292 = CARTESIAN_POINT ( 'NONE',  ( -65.37429515991448170, 15.36281861597759502, -204.5121470880695256 ) ) ;
#293 = DIRECTION ( 'NONE',  ( 0.000000000000000000, 0.000000000000000000, -1.000000000000000000 ) ) ;
#294 = CARTESIAN_POINT ( 'NONE',  ( -2.298097038856279362, 1.874999999999999778, -5.798097038856278473 ) ) ;
#295 = CARTESIAN_POINT ( 'NONE',  ( 6.904992501205359900, 0.03088707369837453628, -105.2571219807955600 ) ) ;
#296 = SHAPE_DEFINITION_REPRESENTATION ( #8175, #10891 ) ;
#297 = PRODUCT_DEFINITION_SHAPE ( 'NONE', 'NONE',  #15318 ) ;
#298 = CARTESIAN_POINT ( 'NONE',  ( -8.289881740238500996, 2.075239479414269894, -35.21986562831451550 ) ) ;
#299 = CARTESIAN_POINT ( 'NONE',  ( 4.554677347145018373, -2.225540348348185052E-17, -1.000000000000000000 ) ) ;
#300 = APPROVAL_PERSON_ORGANIZATION ( #14276, #10653, #10784 ) ;
#301 = ORIENTED_EDGE ( 'NONE', *, *, #10792, .F. ) ;
#302 = CARTESIAN_POINT ( 'NONE',  ( 7.612871144712937799, 1.444594270924061563, 4.322043199100508382 ) ) ;
#303 = CARTESIAN_POINT ( 'NONE',  ( 3.249999999999998668, 6.687500000000000888, -4.846194077712560500 ) ) ;
#304 = CARTESIAN_POINT ( 'NONE',  ( -8.846059151020902789, 1.095509632927770260, -104.9965497395157854 ) ) ;
#305 = CARTESIAN_POINT ( 'NONE',  ( 3.249999999999999556, 1.249999999999999778, -3.500000000000000000 ) ) ;
#306 = CARTESIAN_POINT ( 'NONE',  ( 0.000000000000000000, 9.500000000000000000, -0.2500000000000002220 ) ) ;
#307 = CARTESIAN_POINT ( 'NONE',  ( -5.187227155190234029, 9.999999999999998224, -114.5705604395994044 ) ) ;
#308 = CARTESIAN_POINT ( 'NONE',  ( 1.126705156255721763, 12.88850925732717556, 2.355817795760899447 ) ) ;
#309 = CARTESIAN_POINT ( 'NONE',  ( 9.781835551935063933, 14.76107634091859211, -106.3941254748761764 ) ) ;
#310 = CARTESIAN_POINT ( 'NONE',  ( -1.346194077712559389, 4.062500000000000000, -0.2500000000000002220 ) ) ;
#311 = CARTESIAN_POINT ( 'NONE',  ( 0.000000000000000000, 15.50000000000000178, -0.2500000000000002220 ) ) ;
#312 = CARTESIAN_POINT ( 'NONE',  ( -1.553300858899106407, 7.062500000000000000, 0.2500000000000002220 ) ) ;
#313 = CARTESIAN_POINT ( 'NONE',  ( -3.686354355357802426, 9.944922017739179054, -47.56185035043098708 ) ) ;
#314 = CARTESIAN_POINT ( 'NONE',  ( -3.750000000000000000, 6.812500000000001776, -5.053300858899105741 ) ) ;
#315 = CARTESIAN_POINT ( 'NONE',  ( 3.580916657172306117, 14.85449318919366846, 1.548757939767684721 ) ) ;
#316 = CARTESIAN_POINT ( 'NONE',  ( 10.81319851844414792, 0.4839222075730109651, -164.6269009810859814 ) ) ;
#317 = EDGE_CURVE ( 'NONE', #11237, #8015, #6605, .T. ) ;
#318 = VECTOR ( 'NONE', #638, 1000.000000000000000 ) ;
#319 = CARTESIAN_POINT ( 'NONE',  ( -8.886921396801785278, 2.331427915607008572, -105.5168766094550534 ) ) ;
#320 = EDGE_CURVE ( 'NONE', #2721, #6383, #11005, .T. ) ;
#321 = CARTESIAN_POINT ( 'NONE',  ( -7.527385229589118154, 8.673617379884035472E-16, -152.8686794106570801 ) ) ;
#322 = CARTESIAN_POINT ( 'NONE',  ( 9.068716941525991615, 0.000000000000000000, -163.1923081219560174 ) ) ;
#323 = DIRECTION ( 'NONE',  ( 0.000000000000000000, 0.000000000000000000, -1.000000000000000000 ) ) ;
#324 = CARTESIAN_POINT ( 'NONE',  ( 4.047901358979359543, 5.000000000000000888, -106.4041221358673113 ) ) ;
#325 = ORIENTED_EDGE ( 'NONE', *, *, #7627, .F. ) ;
#326 = CARTESIAN_POINT ( 'NONE',  ( 2.651650429449552870, 9.125000000000000000, -6.151650429449555091 ) ) ;
#327 = ORIENTED_EDGE ( 'NONE', *, *, #13407, .F. ) ;
#328 = CARTESIAN_POINT ( 'NONE',  ( -2.880881586774806546, 8.673617379884035472E-16, -116.0176383781107461 ) ) ;
#329 = CARTESIAN_POINT ( 'NONE',  ( -6.119281984250456219, -2.490287375297126626, -44.38286699775952826 ) ) ;
#330 = CARTESIAN_POINT ( 'NONE',  ( 3.750000000000000000, 9.750000000000000000, -3.500000000000000444 ) ) ;
#331 = CARTESIAN_POINT ( 'NONE',  ( -1.553300858899106629, 7.562500000000000888, 0.2499999999999998335 ) ) ;
#332 = CYLINDRICAL_SURFACE ( 'NONE', #1318, 3.000000000000011990 ) ;
#333 = VERTEX_POINT ( 'NONE', #2504 ) ;
#334 = AXIS2_PLACEMENT_3D ( 'NONE', #907, #6844, #6699 ) ;
#335 = CARTESIAN_POINT ( 'NONE',  ( 1.346194077712561166, 4.437499999999999112, -0.2500000000000011102 ) ) ;
#336 = CARTESIAN_POINT ( 'NONE',  ( 2.651650429449553759, 8.875000000000001776, -0.8483495705504471296 ) ) ;
#337 = CARTESIAN_POINT ( 'NONE',  ( -64.88161843510579274, 15.00000000000000000, -196.1685357079028620 ) ) ;
#338 = DIRECTION ( 'NONE',  ( -0.9510565162951488682, 0.000000000000000000, 0.3090169943749619952 ) ) ;
#339 = DIRECTION ( 'NONE',  ( 0.000000000000000000, 0.000000000000000000, 1.000000000000000000 ) ) ;
#340 = CARTESIAN_POINT ( 'NONE',  ( -1.346194077712559389, 7.437500000000000888, -6.749999999999999112 ) ) ;
#341 = DIRECTION ( 'NONE',  ( 0.000000000000000000, 0.000000000000000000, 1.000000000000000000 ) ) ;
#342 = ADVANCED_FACE ( 'NONE', ( #8359 ), #7831, .T. ) ;
#343 = CARTESIAN_POINT ( 'NONE',  ( -3.608581043498830354, 8.673617379884035472E-16, -119.4283565286392559 ) ) ;
#344 = CARTESIAN_POINT ( 'NONE',  ( 3.623039170307543078, 8.673617379884035472E-16, -110.8080360795144372 ) ) ;
#345 = ORIENTED_EDGE ( 'NONE', *, *, #4027, .T. ) ;
#346 = AXIS2_PLACEMENT_3D ( 'NONE', #9220, #2189, #4657 ) ;
#347 = CARTESIAN_POINT ( 'NONE',  ( -0.2500000000000000555, 5.000000000000000000, -0.2499999999999997780 ) ) ;
#348 = VECTOR ( 'NONE', #4531, 1000.000000000000114 ) ;
#349 = DIRECTION ( 'NONE',  ( 0.000000000000000000, 1.000000000000000000, 0.000000000000000000 ) ) ;
#350 = EDGE_LOOP ( 'NONE', ( #5092, #7181, #10098, #3066 ) ) ;
#351 = ORIENTED_EDGE ( 'NONE', *, *, #9219, .T. ) ;
#352 = FACE_OUTER_BOUND ( 'NONE', #11436, .T. ) ;
#353 = CARTESIAN_POINT ( 'NONE',  ( -2.651650429449552870, 12.62500000000000000, -0.8483495705504467965 ) ) ;
#354 = CARTESIAN_POINT ( 'NONE',  ( 1.346194077712561166, 12.43750000000000000, -0.2500000000000011102 ) ) ;
#355 = CARTESIAN_POINT ( 'NONE',  ( -3.249999999999999112, 11.81250000000000178, -4.846194077712558723 ) ) ;
#356 = ORIENTED_EDGE ( 'NONE', *, *, #13763, .F. ) ;
#357 = LINE ( 'NONE', #12527, #6752 ) ;
#358 = CARTESIAN_POINT ( 'NONE',  ( -1.346194077712559389, 7.062500000000000000, -0.2500000000000002220 ) ) ;
#359 = VECTOR ( 'NONE', #9016, 1000.000000000000227 ) ;
#360 = CC_DESIGN_PERSON_AND_ORGANIZATION_ASSIGNMENT ( #9940, #9079, ( #4203 ) ) ;
#361 = CARTESIAN_POINT ( 'NONE',  ( -25.42287067452675586, 4.143790226087491035, -209.0992770757332835 ) ) ;
#362 = CARTESIAN_POINT ( 'NONE',  ( 4.031205673867843231, 0.1109222935295775953, -0.8398591784643215652 ) ) ;
#363 = CARTESIAN_POINT ( 'NONE',  ( -63.60348060676458459, 15.00000000000000000, -180.2685449772604045 ) ) ;
#364 = APPROVAL_STATUS ( 'not_yet_approved' ) ;
#365 = EDGE_CURVE ( 'NONE', #14267, #13371, #3381, .T. ) ;
#366 = CARTESIAN_POINT ( 'NONE',  ( -24.98815304704661600, 1.710977557088027678, -206.9418329696514718 ) ) ;
#367 = EDGE_CURVE ( 'NONE', #14660, #7693, #12911, .T. ) ;
#368 = EDGE_CURVE ( 'NONE', #9693, #10703, #2656, .T. ) ;
#369 = ORIENTED_EDGE ( 'NONE', *, *, #451, .F. ) ;
#370 = CARTESIAN_POINT ( 'NONE',  ( -3.249999999999999556, 9.250000000000000000, -3.499999999999999556 ) ) ;
#371 = CARTESIAN_POINT ( 'NONE',  ( -3.249999999999999556, 0.1875000000000000278, -2.153805922287440833 ) ) ;
#372 = VECTOR ( 'NONE', #723, 1000.000000000000000 ) ;
#373 = CARTESIAN_POINT ( 'NONE',  ( 3.749999999999999112, 14.81250000000000000, -1.946699141100892039 ) ) ;
#374 = B_SPLINE_CURVE_WITH_KNOTS ( 'NONE', 3,
 ( #12760, #7878, #3398, #5716 ),
 .UNSPECIFIED., .F., .F.,
 ( 4, 4 ),
 ( 0.000000000000000000, 0.01415222705959193195 ),
 .UNSPECIFIED. ) ;
#375 = CARTESIAN_POINT ( 'NONE',  ( -3.616507224213203475, 2.490287375297124850, -0.7961248001406434627 ) ) ;
#376 = CARTESIAN_POINT ( 'NONE',  ( 0.000000000000000000, 1.000000000000000000, 0.2500000000000002220 ) ) ;
#377 = CARTESIAN_POINT ( 'NONE',  ( -67.63566299370725687, 12.50589072862690898, -202.8433208949320488 ) ) ;
#378 = DIRECTION ( 'NONE',  ( -0.002879925520667554837, 0.000000000000000000, -0.9999958530058988826 ) ) ;
#379 = CARTESIAN_POINT ( 'NONE',  ( 8.429434715646030085, 0.4626179564848506565, -105.7324733393003413 ) ) ;
#380 = MECHANICAL_CONTEXT ( 'NONE', #1665, 'mechanical' ) ;
#381 = CARTESIAN_POINT ( 'NONE',  ( -66.58084616437841419, 14.78522502373413694, -192.0328052694261487 ) ) ;
#382 = CARTESIAN_POINT ( 'NONE',  ( 0.000000000000000000, 0.000000000000000000, 0.000000000000000000 ) ) ;
#383 = ORIENTED_EDGE ( 'NONE', *, *, #11565, .F. ) ;
#384 = CARTESIAN_POINT ( 'NONE',  ( 5.231840533899993595, 1.637990804157756664, 3.762912466793266297 ) ) ;
#385 = CARTESIAN_POINT ( 'NONE',  ( 1.346194077712558279, 5.562500000000000000, -6.750000000000000000 ) ) ;
#386 = CARTESIAN_POINT ( 'NONE',  ( -8.867224457307584018, 1.189964233207651878, -104.5821247736135717 ) ) ;
#387 = CARTESIAN_POINT ( 'NONE',  ( -2.298097038856278473, 13.12500000000000000, -1.201902961143720416 ) ) ;
#388 = CARTESIAN_POINT ( 'NONE',  ( 3.249999999999998224, 12.18750000000000178, -4.846194077712561388 ) ) ;
#389 = CARTESIAN_POINT ( 'NONE',  ( -47.48189921986827500, 5.000000000000000000, -141.5723758807981483 ) ) ;
#390 = CYLINDRICAL_SURFACE ( 'NONE', #5044, 3.500000000000000000 ) ;
#391 = CARTESIAN_POINT ( 'NONE',  ( 11.24760135325740507, 13.22314450393356822, -106.7872448694843399 ) ) ;
#392 = CARTESIAN_POINT ( 'NONE',  ( 0.000000000000000000, 6.000000000000000000, -0.2500000000000002220 ) ) ;
#393 = CARTESIAN_POINT ( 'NONE',  ( -3.749999999999999556, 0.7499999999999998890, -3.499999999999999112 ) ) ;
#394 = CARTESIAN_POINT ( 'NONE',  ( 1.553300858899105963, 5.562500000000000000, -7.250000000000000000 ) ) ;
#395 = CARTESIAN_POINT ( 'NONE',  ( -3.954519906357485404, 10.53291419278240149, -44.70356096009636104 ) ) ;
#396 = CARTESIAN_POINT ( 'NONE',  ( 3.749999999999999556, 8.250000000000000000, -3.500000000000000444 ) ) ;
#397 = CARTESIAN_POINT ( 'NONE',  ( 2.135536195681809968, 14.03964673803787377, 3.771597406321472334 ) ) ;
#398 = CARTESIAN_POINT ( 'NONE',  ( -0.2500000000000000555, 4.500000000000000888, 1.500000000000000222 ) ) ;
#399 = LINE ( 'NONE', #5948, #9300 ) ;
#400 = CARTESIAN_POINT ( 'NONE',  ( -1.694477158799985395, 4.000000000000112799, -141.3413698475477815 ) ) ;
#401 = CARTESIAN_POINT ( 'NONE',  ( 2.298097038856279362, 14.87500000000000178, -1.201902961143720860 ) ) ;
#402 = DIRECTION ( 'NONE',  ( -0.000000000000000000, 1.000000000000000000, -0.000000000000000000 ) ) ;
#403 = ORIENTED_EDGE ( 'NONE', *, *, #14661, .F. ) ;
#404 = CARTESIAN_POINT ( 'NONE',  ( 3.249999999999998224, 0.1875000000000000833, -4.846194077712561388 ) ) ;
#405 = ORIENTED_EDGE ( 'NONE', *, *, #6941, .F. ) ;
#406 = CARTESIAN_POINT ( 'NONE',  ( 4.492499072540838689, 0.000000000000000000, -2.611025101989581820 ) ) ;
#407 = CARTESIAN_POINT ( 'NONE',  ( 7.148068729939689447, -2.490287375297126626, -34.56909192082981974 ) ) ;
#408 = CARTESIAN_POINT ( 'NONE',  ( 2.651650429449553759, 7.875000000000000000, -0.8483495705504471296 ) ) ;
#409 = CARTESIAN_POINT ( 'NONE',  ( -4.592425496802573972E-16, 8.000000000000000000, -7.250000000000000000 ) ) ;
#410 = CARTESIAN_POINT ( 'NONE',  ( -17.53857915289978209, 0.8419440609433440637, -129.9988674391065047 ) ) ;
#411 = VERTEX_POINT ( 'NONE', #1650 ) ;
#412 = EDGE_CURVE ( 'NONE', #5516, #2826, #7749, .T. ) ;
#413 = CARTESIAN_POINT ( 'NONE',  ( 2.298097038856278029, 6.125000000000000000, -5.798097038856279362 ) ) ;
#414 = CARTESIAN_POINT ( 'NONE',  ( 2.651650429449552870, 11.62500000000000000, -6.151650429449554203 ) ) ;
#415 = CARTESIAN_POINT ( 'NONE',  ( -69.57949925788119572, 9.999999999999998224, -184.9351518006301660 ) ) ;
#416 = LINE ( 'NONE', #571, #1497 ) ;
#417 = DATE_AND_TIME ( #1718, #14648 ) ;
#418 = CARTESIAN_POINT ( 'NONE',  ( -3.249999999999999556, 7.250000000000000000, -3.499999999999999556 ) ) ;
#419 = CARTESIAN_POINT ( 'NONE',  ( -8.589347325610479089, 9.999999999999184652, -120.3237211899656955 ) ) ;
#420 = PERSON_AND_ORGANIZATION ( #7779, #10369 ) ;
#421 = CARTESIAN_POINT ( 'NONE',  ( -9.247150027884355694, 4.999999999998421707, -118.2023151954170288 ) ) ;
#422 = CARTESIAN_POINT ( 'NONE',  ( 3.734989709506049138, 8.673617379884035472E-16, -110.3183269162431230 ) ) ;
#423 = ORIENTED_EDGE ( 'NONE', *, *, #468, .F. ) ;
#424 = CARTESIAN_POINT ( 'NONE',  ( -29.69515346086420138, 15.00000000000000000, -156.7390981038714983 ) ) ;
#425 = CARTESIAN_POINT ( 'NONE',  ( 10.96506291612846162, 11.77387593150068668, -44.79863320250961323 ) ) ;
#426 = ORIENTED_EDGE ( 'NONE', *, *, #15123, .F. ) ;
#427 = ORIENTED_EDGE ( 'NONE', *, *, #7782, .T. ) ;
#428 = PERSON ( 'NAUO-PER7', 'UNSPECIFIED', 'UNSPECIFIED', ('UNSPECIFIED'), ('UNSPECIFIED'), ('UNSPECIFIED') ) ;
#429 = DIRECTION ( 'NONE',  ( -0.000000000000000000, 1.000000000000000000, -0.000000000000000000 ) ) ;
#430 = CARTESIAN_POINT ( 'NONE',  ( 1.553300858899105963, 11.06250000000000178, -7.249999999999999112 ) ) ;
#431 = CARTESIAN_POINT ( 'NONE',  ( -3.249999999999999112, 11.68749999999999822, -2.153805922287440833 ) ) ;
#432 = CARTESIAN_POINT ( 'NONE',  ( 2.298097038856279362, 12.37500000000000178, -1.201902961143720860 ) ) ;
#433 = ADVANCED_FACE ( 'NONE', ( #13637 ), #3589, .F. ) ;
#434 = EDGE_LOOP ( 'NONE', ( #13261, #4707, #9189, #5976 ) ) ;
#435 = LINE ( 'NONE', #7296, #14161 ) ;
#436 =( BOUNDED_CURVE ( )  B_SPLINE_CURVE ( 3, ( #14135, #7607, #10719, #6304 ),
 .UNSPECIFIED., .F., .F. ) 
 B_SPLINE_CURVE_WITH_KNOTS ( ( 4, 4 ),
 ( 1.570796326794899667, 1.765402715644074361 ),
 .UNSPECIFIED. ) 
 CURVE ( )  GEOMETRIC_REPRESENTATION_ITEM ( )  RATIONAL_B_SPLINE_CURVE ( ( 1.000000000000000000, 0.9968465187034001307, 0.9968465187034001307, 1.000000000000000000 ) ) 
 REPRESENTATION_ITEM ( '' )  );
#437 = CARTESIAN_POINT ( 'NONE',  ( 1.346194077712560944, 6.937500000000000000, -0.2500000000000010547 ) ) ;
#438 = EDGE_CURVE ( 'NONE', #15209, #13242, #13713, .T. ) ;
#439 = CARTESIAN_POINT ( 'NONE',  ( 1.078198036487820088, 5.000000000000000888, -139.4303465535634245 ) ) ;
#440 = CARTESIAN_POINT ( 'NONE',  ( -36.44277747304521853, 10.00000000000000355, -156.3629325348109376 ) ) ;
#441 = FACE_OUTER_BOUND ( 'NONE', #3722, .T. ) ;
#442 = APPROVAL_ROLE ( '' ) ;
#443 = CARTESIAN_POINT ( 'NONE',  ( -0.3766621274091715432, -0.2054769798019681903, -0.1347136637304948981 ) ) ;
#444 = ORIENTED_EDGE ( 'NONE', *, *, #15170, .F. ) ;
#445 = CARTESIAN_POINT ( 'NONE',  ( -3.249999999999999556, 1.187500000000000444, -2.153805922287440833 ) ) ;
#446 = CARTESIAN_POINT ( 'NONE',  ( 3.749999999999999112, 12.81250000000000000, -1.946699141100892039 ) ) ;
#447 = VERTEX_POINT ( 'NONE', #7825 ) ;
#448 = CARTESIAN_POINT ( 'NONE',  ( -4.878690035801932723, 1.020558061026469066, -0.3860167444088121180 ) ) ;
#449 = ADVANCED_FACE ( 'NONE', ( #4058 ), #14960, .T. ) ;
#450 = CARTESIAN_POINT ( 'NONE',  ( -3.749999999999999556, 0.1875000000000001110, -1.946699141100892927 ) ) ;
#451 = EDGE_CURVE ( 'NONE', #887, #14484, #14806, .T. ) ;
#452 = CARTESIAN_POINT ( 'NONE',  ( 6.436143463598923198, 9.999999999999998224, 2.800833825385760090 ) ) ;
#453 = DIRECTION ( 'NONE',  ( 0.000000000000000000, -0.000000000000000000, 1.000000000000000000 ) ) ;
#454 = CARTESIAN_POINT ( 'NONE',  ( 11.01414178047344095, 4.315957715773897974, -107.1012222462659196 ) ) ;
#455 = PERSON_AND_ORGANIZATION ( #3176, #3020 ) ;
#456 = CARTESIAN_POINT ( 'NONE',  ( -67.58382170693633384, 10.13932288468602039, -204.5178482451962338 ) ) ;
#457 = DIRECTION ( 'NONE',  ( -0.000000000000000000, -1.000000000000000000, -0.000000000000000000 ) ) ;
#458 = ORIENTED_EDGE ( 'NONE', *, *, #10462, .T. ) ;
#459 = CARTESIAN_POINT ( 'NONE',  ( -3.249999999999999556, 8.312500000000000000, -4.846194077712557835 ) ) ;
#460 = CARTESIAN_POINT ( 'NONE',  ( -8.133653642740192424, 0.3980376946237794700, -104.7021510399676174 ) ) ;
#461 = CARTESIAN_POINT ( 'NONE',  ( 3.249999999999998668, 12.68750000000000178, -4.846194077712560500 ) ) ;
#462 = CARTESIAN_POINT ( 'NONE',  ( 3.249999999999998224, 9.187500000000001776, -4.846194077712561388 ) ) ;
#463 = CARTESIAN_POINT ( 'NONE',  ( -8.605705957304479625, 14.99999999998180122, -105.7466801460949171 ) ) ;
#464 = CARTESIAN_POINT ( 'NONE',  ( 7.432103217121470706, 5.104710470816895551, -26.33708262891812879 ) ) ;
#465 = CARTESIAN_POINT ( 'NONE',  ( 10.67045167996756128, 14.18553633651329804, -106.2656505685997104 ) ) ;
#466 = CARTESIAN_POINT ( 'NONE',  ( -2.298097038856278918, 5.375000000000000000, -5.798097038856277585 ) ) ;
#467 = CARTESIAN_POINT ( 'NONE',  ( 3.749999999999999556, 7.250000000000000000, -3.500000000000000444 ) ) ;
#468 = EDGE_CURVE ( 'NONE', #1674, #6553, #14959, .T. ) ;
#469 = CARTESIAN_POINT ( 'NONE',  ( 2.651650429449552870, 7.625000000000000000, -6.151650429449554203 ) ) ;
#470 = CARTESIAN_POINT ( 'NONE',  ( 0.1113706952913113279, 2.624400893789762268, 1.261497925137973652 ) ) ;
#471 = CARTESIAN_POINT ( 'NONE',  ( 2.651650429449554203, 9.374999999999998224, -0.8483495705504471296 ) ) ;
#472 = DIRECTION ( 'NONE',  ( 0.000000000000000000, 0.000000000000000000, 1.000000000000000000 ) ) ;
#473 = CARTESIAN_POINT ( 'NONE',  ( 12.49422757225345570, 2.167092202804963730, -165.7027478962374971 ) ) ;
#474 = CARTESIAN_POINT ( 'NONE',  ( -4.507463604512252253, 5.000000000000000000, -2.585105772303598393 ) ) ;
#475 = CARTESIAN_POINT ( 'NONE',  ( -8.055328022171806879, 8.673617379884035472E-16, -153.4262481318472737 ) ) ;
#476 = CARTESIAN_POINT ( 'NONE',  ( 6.577825583858426306, 0.000000000000000000, -139.0000488628143103 ) ) ;
#477 = CARTESIAN_POINT ( 'NONE',  ( -25.40168623993593400, 8.673617379884045333E-16, -197.6107370494183044 ) ) ;
#478 = EDGE_LOOP ( 'NONE', ( #9570, #4632, #3133, #10760 ) ) ;
#479 = CARTESIAN_POINT ( 'NONE',  ( -3.249999999999999112, -0.3124999999999999445, -2.153805922287440833 ) ) ;
#480 = ORIENTED_EDGE ( 'NONE', *, *, #12357, .T. ) ;
#481 = DIRECTION ( 'NONE',  ( 0.000000000000000000, -0.9434476287765544145, 0.3315216007380165641 ) ) ;
#482 = CARTESIAN_POINT ( 'NONE',  ( -19.28976728528864371, 4.000000000000588862, -198.7222929113018779 ) ) ;
#483 = CARTESIAN_POINT ( 'NONE',  ( -1.553300858899106629, 7.062500000000000000, 0.2500000000000002220 ) ) ;
#484 = CARTESIAN_POINT ( 'NONE',  ( -1.553300858899106629, 9.562500000000000000, 0.2499999999999998335 ) ) ;
#485 = CARTESIAN_POINT ( 'NONE',  ( -3.625354560620934752, 10.18683717591091842, -47.21077240160808230 ) ) ;
#486 = ORIENTED_EDGE ( 'NONE', *, *, #6759, .F. ) ;
#487 = CARTESIAN_POINT ( 'NONE',  ( 2.298097038856279362, 10.37500000000000000, -1.201902961143720860 ) ) ;
#488 = CARTESIAN_POINT ( 'NONE',  ( -1.553300858899107295, 8.437500000000000000, -7.250000000000000000 ) ) ;
#489 = CARTESIAN_POINT ( 'NONE',  ( -65.08324626441498140, 15.00000000000000000, -193.5244750848175386 ) ) ;
#490 = PERSON_AND_ORGANIZATION_ROLE ( 'creator' ) ;
#491 = CARTESIAN_POINT ( 'NONE',  ( 1.346194077712560944, 8.937500000000001776, -0.2500000000000010547 ) ) ;
#492 = CARTESIAN_POINT ( 'NONE',  ( -0.7011654427748897911, 2.490287375297123962, -44.24552462515097773 ) ) ;
#493 = LOCAL_TIME ( 12, 28, 20.00000000000000000, #7069 ) ;
#494 = CARTESIAN_POINT ( 'NONE',  ( 0.000000000000000000, 5.000000000000000000, 0.000000000000000000 ) ) ;
#495 = CARTESIAN_POINT ( 'NONE',  ( 3.361270396691331541, 8.673617379884035472E-16, -115.2606357392248242 ) ) ;
#496 = VECTOR ( 'NONE', #13337, 1000.000000000000000 ) ;
#497 = FACE_OUTER_BOUND ( 'NONE', #2057, .T. ) ;
#498 = CARTESIAN_POINT ( 'NONE',  ( 10.95172361697086139, 11.63674386448545128, -43.69557350477573010 ) ) ;
#499 = ORIENTED_EDGE ( 'NONE', *, *, #8183, .T. ) ;
#500 = CARTESIAN_POINT ( 'NONE',  ( 10.00087860767147241, 5.000000000000001776, -45.95880046359210525 ) ) ;
#501 = CARTESIAN_POINT ( 'NONE',  ( 7.347880794884122694E-16, 1.000000000000000000, 6.000000000000002665 ) ) ;
#502 = CARTESIAN_POINT ( 'NONE',  ( -2.651650429449552870, 10.62500000000000178, -0.8483495705504467965 ) ) ;
#503 = CARTESIAN_POINT ( 'NONE',  ( 0.000000000000000000, 9.500000000000001776, -0.2500000000000002220 ) ) ;
#504 = CARTESIAN_POINT ( 'NONE',  ( 1.346194077712558057, 1.562500000000000000, -6.750000000000000000 ) ) ;
#505 = VERTEX_POINT ( 'NONE', #10446 ) ;
#506 = CARTESIAN_POINT ( 'NONE',  ( -3.249999999999999556, 7.250000000000000000, -3.499999999999999556 ) ) ;
#507 = LOCAL_TIME ( 12, 28, 20.00000000000000000, #960 ) ;
#508 = CARTESIAN_POINT ( 'NONE',  ( -47.48189921986828210, 15.00000000000000000, -141.5723758807981483 ) ) ;
#509 = AXIS2_PLACEMENT_3D ( 'NONE', #9059, #10445, #12537 ) ;
#510 = CARTESIAN_POINT ( 'NONE',  ( 9.958926971456385502, 12.69564389515387326, -44.38794094253861999 ) ) ;
#511 = CARTESIAN_POINT ( 'NONE',  ( 0.000000000000000000, 5.000000000000000000, -3.500000000000000000 ) ) ;
#512 = DIRECTION ( 'NONE',  ( 0.000000000000000000, 1.000000000000000000, 0.000000000000000000 ) ) ;
#513 = CALENDAR_DATE ( 2026, 8, 10 ) ;
#514 = DIRECTION ( 'NONE',  ( 0.000000000000000000, 0.000000000000000000, -1.000000000000000000 ) ) ;
#515 = CIRCLE ( 'NONE', #2242, 5.000000000000002665 ) ;
#516 = ORIENTED_EDGE ( 'NONE', *, *, #2307, .T. ) ;
#517 = EDGE_CURVE ( 'NONE', #14224, #673, #14001, .T. ) ;
#518 = CARTESIAN_POINT ( 'NONE',  ( -3.980102097228897245E-16, 0.5000000000000000000, -6.749999999999999112 ) ) ;
#519 = CARTESIAN_POINT ( 'NONE',  ( -1.553300858899107295, 12.43750000000000000, -7.250000000000000000 ) ) ;
#520 = AXIS2_PLACEMENT_3D ( 'NONE', #7871, #1136, #702 ) ;
#521 = EDGE_LOOP ( 'NONE', ( #12296, #11775, #1028, #6715 ) ) ;
#522 = CARTESIAN_POINT ( 'NONE',  ( -4.422205167688408878, 1.921202954650395256, -0.5343376690911894045 ) ) ;
#523 = CARTESIAN_POINT ( 'NONE',  ( 3.749999999999998668, 1.687500000000000000, -5.053300858899107517 ) ) ;
#524 = CARTESIAN_POINT ( 'NONE',  ( -5.445322652854981627, 5.900679960901947346E-16, -1.000000000000000000 ) ) ;
#525 = CARTESIAN_POINT ( 'NONE',  ( 3.211135607724114660, 3.697509922049161180, 5.038955779812875235 ) ) ;
#526 = CARTESIAN_POINT ( 'NONE',  ( -5.309262520577839872, 6.000000000000000000, -125.0911079416483176 ) ) ;
#527 = CIRCLE ( 'NONE', #15081, 2.000000000000016431 ) ;
#528 = CALENDAR_DATE ( 2026, 8, 10 ) ;
#529 = CARTESIAN_POINT ( 'NONE',  ( -3.578160823487617215, 2.490287375297123518, -0.5540151544771234615 ) ) ;
#530 = CARTESIAN_POINT ( 'NONE',  ( 3.902875325215932723, 12.49999999999999822, -114.6800873586639824 ) ) ;
#531 = EDGE_LOOP ( 'NONE', ( #11710, #5014, #10562, #10714 ) ) ;
#532 = EDGE_CURVE ( 'NONE', #7071, #4481, #12762, .T. ) ;
#533 = CARTESIAN_POINT ( 'NONE',  ( -3.249999999999999556, 7.250000000000000000, -3.499999999999999556 ) ) ;
#534 = EDGE_CURVE ( 'NONE', #8407, #5461, #13303, .T. ) ;
#535 = DIRECTION ( 'NONE',  ( 0.6182966555592912528, 0.000000000000000000, 0.7859448108640934016 ) ) ;
#536 = CARTESIAN_POINT ( 'NONE',  ( 3.249999999999998224, 1.312500000000000000, -2.153805922287439945 ) ) ;
#537 = VECTOR ( 'NONE', #8626, 1000.000000000000000 ) ;
#538 = CARTESIAN_POINT ( 'NONE',  ( 2.298097038856279362, 11.37500000000000000, -1.201902961143720860 ) ) ;
#539 = CARTESIAN_POINT ( 'NONE',  ( -8.605705957300969544, 9.999999999999998224, -105.7466801460984840 ) ) ;
#540 = CARTESIAN_POINT ( 'NONE',  ( -11.47368464600194571, 2.500000000000000444, -126.3895689751090856 ) ) ;
#541 = CARTESIAN_POINT ( 'NONE',  ( 3.249999999999999556, 4.750000000000000000, -3.500000000000000000 ) ) ;
#542 = CARTESIAN_POINT ( 'NONE',  ( -2.651650429449552870, 5.875000000000000888, -6.151650429449552426 ) ) ;
#543 = CARTESIAN_POINT ( 'NONE',  ( -1.553300858899106407, 11.06250000000000000, 0.2500000000000002220 ) ) ;
#544 = DIRECTION ( 'NONE',  ( -0.000000000000000000, -1.000000000000000000, -0.000000000000000000 ) ) ;
#545 = CARTESIAN_POINT ( 'NONE',  ( -3.625372539825013618, 10.18678395325208719, -47.21086670346684855 ) ) ;
#546 = CARTESIAN_POINT ( 'NONE',  ( 0.000000000000000000, 8.500000000000000000, 0.2500000000000002220 ) ) ;
#547 = CARTESIAN_POINT ( 'NONE',  ( 4.900580087367143456, 14.89515687054757365, -1.231267350884497125 ) ) ;
#548 = APPROVAL ( #10469, 'UNKNOWN' ) ;
#549 = CC_DESIGN_APPROVAL ( #8378, ( #7950 ) ) ;
#550 = CARTESIAN_POINT ( 'NONE',  ( 12.35274956116099254, 1.933739209396013514, -165.5990192671287105 ) ) ;
#551 = CARTESIAN_POINT ( 'NONE',  ( 29.71057115341584165, 0.000000000000000000, 36.39324188472025412 ) ) ;
#552 = EDGE_CURVE ( 'NONE', #6914, #4341, #15183, .T. ) ;
#553 = CARTESIAN_POINT ( 'NONE',  ( -17.27880384526778101, 1.734723475976807094E-15, -165.6175314860322771 ) ) ;
#554 = CARTESIAN_POINT ( 'NONE',  ( 3.235167919141237913, 8.673617379884037444E-16, -114.6791120453068942 ) ) ;
#555 = EDGE_CURVE ( 'NONE', #12741, #14503, #11276, .T. ) ;
#556 = CARTESIAN_POINT ( 'NONE',  ( -39.01706460773457508, 9.999999999999998224, -156.9624841732276650 ) ) ;
#557 = EDGE_CURVE ( 'NONE', #4897, #14271, #1403, .T. ) ;
#558 = CARTESIAN_POINT ( 'NONE',  ( 1.553300858899109516, 12.43750000000000000, 0.2499999999999993616 ) ) ;
#559 = VERTEX_POINT ( 'NONE', #11746 ) ;
#560 = CARTESIAN_POINT ( 'NONE',  ( 13.47730208875211844, 6.000000000000000000, -127.1728814958210876 ) ) ;
#561 = CARTESIAN_POINT ( 'NONE',  ( 6.941279403247599511, 5.883355326356809467E-13, -105.1775688070215438 ) ) ;
#562 = CARTESIAN_POINT ( 'NONE',  ( -2.651650429449552870, 11.12500000000000000, -0.8483495705504462414 ) ) ;
#563 = CARTESIAN_POINT ( 'NONE',  ( 1.553300858899105963, 9.062500000000003553, -7.249999999999999112 ) ) ;
#564 = CARTESIAN_POINT ( 'NONE',  ( -3.315923205871632362, 9.650666666666662508, -43.24506100211545601 ) ) ;
#565 = LOCAL_TIME ( 12, 28, 20.00000000000000000, #3217 ) ;
#566 = CARTESIAN_POINT ( 'NONE',  ( -9.385448346790807861, 4.636404319127126250, -115.3551636526218687 ) ) ;
#567 = CARTESIAN_POINT ( 'NONE',  ( -1.346194077712559167, 7.937500000000001776, -6.749999999999999112 ) ) ;
#568 = CARTESIAN_POINT ( 'NONE',  ( 1.553300858899105963, 0.06250000000000016653, -7.250000000000000888 ) ) ;
#569 = AXIS2_PLACEMENT_3D ( 'NONE', #10282, #10214, #3101 ) ;
#570 = DIRECTION ( 'NONE',  ( -0.000000000000000000, -1.000000000000000000, -0.000000000000000000 ) ) ;
#571 = CARTESIAN_POINT ( 'NONE',  ( -0.3766621274091715987, -0.2500000000000000000, 0.1491815183709511716 ) ) ;
#572 = DIRECTION ( 'NONE',  ( 0.000000000000000000, 0.000000000000000000, 1.000000000000000000 ) ) ;
#573 = CARTESIAN_POINT ( 'NONE',  ( -3.980102097228897245E-16, 13.50000000000000000, -6.749999999999999112 ) ) ;
#574 = CARTESIAN_POINT ( 'NONE',  ( -5.899062623765880531, 10.00000000000000178, -109.4162288830486887 ) ) ;
#575 = FACE_OUTER_BOUND ( 'NONE', #10280, .T. ) ;
#576 = CARTESIAN_POINT ( 'NONE',  ( 11.18419171849477323, 5.000000000000000888, -106.9754176129513752 ) ) ;
#577 = CARTESIAN_POINT ( 'NONE',  ( -6.790153584124027475, 6.000000000000000000, -124.9643354754709748 ) ) ;
#578 = CARTESIAN_POINT ( 'NONE',  ( 0.000000000000000000, 1.530808498934191509E-17, 0.000000000000000000 ) ) ;
#579 = ORIENTED_EDGE ( 'NONE', *, *, #14346, .F. ) ;
#580 = CARTESIAN_POINT ( 'NONE',  ( 10.98638911170980670, 5.830450750434273743, -45.28397108166865337 ) ) ;
#581 = CARTESIAN_POINT ( 'NONE',  ( 11.97422441543835525, 12.49999999999999289, -123.6845202709325520 ) ) ;
#582 = CARTESIAN_POINT ( 'NONE',  ( 3.749999999999998668, 14.18750000000000178, -5.053300858899108405 ) ) ;
#583 = CIRCLE ( 'NONE', #13426, 2.499999999999999556 ) ;
#584 = CARTESIAN_POINT ( 'NONE',  ( -3.249999999999999556, 10.75000000000000178, -3.500000000000000000 ) ) ;
#585 = CC_DESIGN_DATE_AND_TIME_ASSIGNMENT ( #6865, #8027, ( #9258 ) ) ;
#586 = CARTESIAN_POINT ( 'NONE',  ( 0.000000000000000000, 0.000000000000000000, -0.2500000000000002220 ) ) ;
#587 = VERTEX_POINT ( 'NONE', #5869 ) ;
#588 = CARTESIAN_POINT ( 'NONE',  ( -1.346194077712559389, 9.437500000000000000, -6.749999999999999112 ) ) ;
#589 = CARTESIAN_POINT ( 'NONE',  ( -1.500000000000000000, 4.500000000000000888, -0.2499999999999997780 ) ) ;
#590 = APPLICATION_CONTEXT ( 'configuration controlled 3d designs of mechanical parts and assemblies' ) ;
#591 = CARTESIAN_POINT ( 'NONE',  ( -7.079750767422662960, 14.09909992734707807, -104.2797251405894912 ) ) ;
#592 = CARTESIAN_POINT ( 'NONE',  ( 4.804596213718521192, 0.9953211363309286686, 2.828019302905943722 ) ) ;
#593 = CARTESIAN_POINT ( 'NONE',  ( 26.88777289245741642, 6.000000000000000000, -138.4814624290441429 ) ) ;
#594 = CIRCLE ( 'NONE', #14916, 5.000000000000001776 ) ;
#595 = SECURITY_CLASSIFICATION_LEVEL ( 'unclassified' ) ;
#596 = CIRCLE ( 'NONE', #7496, 3.000000000000002665 ) ;
#597 = B_SPLINE_CURVE_WITH_KNOTS ( 'NONE', 3,
 ( #4870, #5, #5800, #3637, #10670, #8499, #9511, #10745, #13150, #1321, #14236, #8339, #14163, #11896, #231, #13064, #10520, #15255 ),
 .UNSPECIFIED., .F., .F.,
 ( 4, 2, 2, 2, 2, 2, 2, 2, 4 ),
 ( 7.806255641895631925E-18, 0.0007604115106050202957, 0.001520823021210032785, 0.002281234531815045166, 0.003041646042420057764, 0.003802057553025070362, 0.004562469063630082526, 0.005322880574235095558, 0.006083292084840107722 ),
 .UNSPECIFIED. ) ;
#598 = DIRECTION ( 'NONE',  ( -0.9961255586397056438, 0.000000000000000000, 0.08794243244722428632 ) ) ;
#599 = EDGE_LOOP ( 'NONE', ( #3826, #9848, #1789, #6970, #3305, #177 ) ) ;
#600 = CARTESIAN_POINT ( 'NONE',  ( -3.249999999999999556, 5.187500000000001776, -2.153805922287440833 ) ) ;
#601 = CARTESIAN_POINT ( 'NONE',  ( 2.651650429449552870, 12.62500000000000000, -6.151650429449554203 ) ) ;
#602 = VERTEX_POINT ( 'NONE', #2107 ) ;
#603 = CARTESIAN_POINT ( 'NONE',  ( -9.030574454602195544, 2.490287375297124850, -34.97919997656152447 ) ) ;
#604 = AXIS2_PLACEMENT_3D ( 'NONE', #5543, #14991, #4390 ) ;
#605 = CIRCLE ( 'NONE', #6521, 6.000000000000002665 ) ;
#606 = ADVANCED_FACE ( 'NONE', ( #6812 ), #11530, .F. ) ;
#607 = CARTESIAN_POINT ( 'NONE',  ( -2.651650429449552870, 0.1250000000000000278, -0.8483495705504462414 ) ) ;
#608 = CARTESIAN_POINT ( 'NONE',  ( 7.251665800977816545, 3.308594936348907112, -24.41847810565704080 ) ) ;
#609 = CARTESIAN_POINT ( 'NONE',  ( 0.4577222846077236285, 2.652767234986340927, 5.184628782367975752 ) ) ;
#610 = CARTESIAN_POINT ( 'NONE',  ( -5.794432043291358525, 6.000000000000000000, -125.0404107129116085 ) ) ;
#611 = APPROVAL_DATE_TIME ( #4317, #1853 ) ;
#612 = DIRECTION ( 'NONE',  ( -1.000000000000000000, 0.000000000000000000, 0.000000000000000000 ) ) ;
#613 = CIRCLE ( 'NONE', #14450, 7.000000000000016875 ) ;
#614 = LINE ( 'NONE', #5091, #1247 ) ;
#615 = ORIENTED_EDGE ( 'NONE', *, *, #2812, .F. ) ;
#616 = CARTESIAN_POINT ( 'NONE',  ( -2.298097038856278918, 9.375000000000000000, -5.798097038856277585 ) ) ;
#617 = DIRECTION ( 'NONE',  ( 0.000000000000000000, 0.000000000000000000, -1.000000000000000000 ) ) ;
#618 = CARTESIAN_POINT ( 'NONE',  ( -3.980102097228897738E-16, 5.000000000000000000, -6.749999999999999112 ) ) ;
#619 = CARTESIAN_POINT ( 'NONE',  ( 3.249999999999998224, 10.31250000000000000, -2.153805922287439945 ) ) ;
#620 = LINE ( 'NONE', #2862, #3306 ) ;
#621 = CARTESIAN_POINT ( 'NONE',  ( 11.24846813935491596, 13.18102764301277219, -106.3932454387446285 ) ) ;
#622 = CARTESIAN_POINT ( 'NONE',  ( 1.346194077712560944, 4.937500000000001776, -0.2500000000000010547 ) ) ;
#623 = CARTESIAN_POINT ( 'NONE',  ( -1.553300858899106629, 4.562500000000000000, 0.2499999999999998335 ) ) ;
#624 = CARTESIAN_POINT ( 'NONE',  ( 2.651650429449552870, 10.62500000000000000, -6.151650429449554203 ) ) ;
#625 = EDGE_CURVE ( 'NONE', #10703, #14402, #14164, .T. ) ;
#626 = LINE ( 'NONE', #13538, #7670 ) ;
#627 = CARTESIAN_POINT ( 'NONE',  ( -7.472766077161563381, 0.9471434298996047607, -116.8715385114339966 ) ) ;
#628 = CARTESIAN_POINT ( 'NONE',  ( -1.553300858899106629, 10.56249999999999822, 0.2500000000000002220 ) ) ;
#629 = CARTESIAN_POINT ( 'NONE',  ( 4.394544305604815015, 15.00077533664657636, -1.522866948741665727 ) ) ;
#630 = CARTESIAN_POINT ( 'NONE',  ( 7.352489943804302541, -2.075239479414269894, -39.38380306805898101 ) ) ;
#631 = DIRECTION ( 'NONE',  ( 0.7260798585963988971, 0.000000000000000000, 0.6876103830954222174 ) ) ;
#632 = CARTESIAN_POINT ( 'NONE',  ( -21.40529191659825159, 8.673617379884035472E-16, -173.7943469130565290 ) ) ;
#633 = CARTESIAN_POINT ( 'NONE',  ( 12.76858567064540217, 3.999999999993260502, -166.6103056774037441 ) ) ;
#634 = UNCERTAINTY_MEASURE_WITH_UNIT (LENGTH_MEASURE( 1.000000000000000082E-05 ), #8357, 'distance_accuracy_value', 'NONE');
#635 = CARTESIAN_POINT ( 'NONE',  ( -39.10933222484039362, 15.00000000000000000, -151.7704989434176923 ) ) ;
#636 = CARTESIAN_POINT ( 'NONE',  ( 1.553300858899105963, 12.06250000000000000, -7.250000000000000888 ) ) ;
#637 = ORIENTED_EDGE ( 'NONE', *, *, #12424, .T. ) ;
#638 = DIRECTION ( 'NONE',  ( -0.000000000000000000, -1.000000000000000000, -0.000000000000000000 ) ) ;
#639 = CARTESIAN_POINT ( 'NONE',  ( 1.831246893856136593, -2.490287375297125294, -1.000000000000021760 ) ) ;
#640 = CARTESIAN_POINT ( 'NONE',  ( 3.749999999999999556, 10.25000000000000178, -3.500000000000000444 ) ) ;
#641 = FACE_OUTER_BOUND ( 'NONE', #434, .T. ) ;
#642 = CARTESIAN_POINT ( 'NONE',  ( 0.000000000000000000, 8.500000000000000000, -0.2500000000000002220 ) ) ;
#643 = ADVANCED_FACE ( 'NONE', ( #2562 ), #1239, .T. ) ;
#644 = CARTESIAN_POINT ( 'NONE',  ( 3.554677347145018373, -2.225540348348185052E-17, 1.000000000000000000 ) ) ;
#645 = CARTESIAN_POINT ( 'NONE',  ( -3.749999999999999556, 13.31250000000000000, -5.053300858899104853 ) ) ;
#646 = FACE_OUTER_BOUND ( 'NONE', #14205, .T. ) ;
#647 = EDGE_CURVE ( 'NONE', #6217, #2052, #399, .T. ) ;
#648 = EDGE_CURVE ( 'NONE', #13215, #10636, #6120, .T. ) ;
#649 = CARTESIAN_POINT ( 'NONE',  ( 3.158384440324541131, 1.020558061026468177, -1.000000000000027311 ) ) ;
#650 = CARTESIAN_POINT ( 'NONE',  ( -3.249999999999999556, 10.31250000000000000, -4.846194077712557835 ) ) ;
#651 = CARTESIAN_POINT ( 'NONE',  ( -8.289881740238515206, 2.529993217055222843, -35.21986562831452261 ) ) ;
#652 = CARTESIAN_POINT ( 'NONE',  ( -1.346194077712559389, 11.06250000000000000, -0.2500000000000002220 ) ) ;
#653 = DIRECTION ( 'NONE',  ( 1.000000000000000000, 0.000000000000000000, -0.000000000000000000 ) ) ;
#654 = CARTESIAN_POINT ( 'NONE',  ( 8.322646197901347520, 2.167618682171565639E-13, -114.4990917221396103 ) ) ;
#655 = FACE_OUTER_BOUND ( 'NONE', #9245, .T. ) ;
#656 = ORIENTED_EDGE ( 'NONE', *, *, #3653, .T. ) ;
#657 = CARTESIAN_POINT ( 'NONE',  ( 10.01221399140626644, 5.773894451085546997, -44.97775305520311662 ) ) ;
#658 = CARTESIAN_POINT ( 'NONE',  ( 4.999999999999998224, 15.00000000000000178, -101.4583377608209389 ) ) ;
#659 = CARTESIAN_POINT ( 'NONE',  ( 2.651650429449552870, 2.625000000000000000, -6.151650429449554203 ) ) ;
#660 = CARTESIAN_POINT ( 'NONE',  ( -1.346194077712558945, 12.56250000000000355, -0.2500000000000002220 ) ) ;
#661 = CARTESIAN_POINT ( 'NONE',  ( 3.249999999999999112, 0.8125000000000001110, -2.153805922287439945 ) ) ;
#662 = ORIENTED_EDGE ( 'NONE', *, *, #10644, .T. ) ;
#663 = CARTESIAN_POINT ( 'NONE',  ( 0.000000000000000000, 11.00000000000000000, -0.2500000000000002220 ) ) ;
#664 = CARTESIAN_POINT ( 'NONE',  ( 10.99551757066059032, 11.56847231179307656, -45.70224318734323532 ) ) ;
#665 = EDGE_CURVE ( 'NONE', #7526, #1605, #6267, .T. ) ;
#666 = CARTESIAN_POINT ( 'NONE',  ( -6.438219714322270804, 14.38465807372143956, -104.2571274176714553 ) ) ;
#667 = CARTESIAN_POINT ( 'NONE',  ( 4.736400576334578005, 0.9069609750089387967, 2.656850315087319281 ) ) ;
#668 = APPROVAL ( #10413, 'UNSPECIFIED' ) ;
#669 = CARTESIAN_POINT ( 'NONE',  ( 27.03835354040190708, 6.000000000000000000, -138.2189567750509696 ) ) ;
#670 = DATE_TIME_ROLE ( 'classification_date' ) ;
#671 = CARTESIAN_POINT ( 'NONE',  ( 13.66360635606377905, 12.49999999999999822, -125.8738101254713513 ) ) ;
#672 = CARTESIAN_POINT ( 'NONE',  ( 26.71007981189074343, 4.606906972201797679, -136.8791680518442320 ) ) ;
#673 = VERTEX_POINT ( 'NONE', #14309 ) ;
#674 = CARTESIAN_POINT ( 'NONE',  ( -3.249999999999999556, 6.312500000000000888, -4.846194077712557835 ) ) ;
#675 = DIRECTION ( 'NONE',  ( 0.000000000000000000, 0.000000000000000000, -1.000000000000000000 ) ) ;
#676 = CARTESIAN_POINT ( 'NONE',  ( -4.592425496802573972E-16, 2.000000000000000000, -7.250000000000000000 ) ) ;
#677 = AXIS2_PLACEMENT_3D ( 'NONE', #6, #9437, #944 ) ;
#678 = ORIENTED_EDGE ( 'NONE', *, *, #14167, .T. ) ;
#679 = CARTESIAN_POINT ( 'NONE',  ( -8.817544209126937815, 12.32420660420548764, -115.6114935513795103 ) ) ;
#680 = CARTESIAN_POINT ( 'NONE',  ( -3.749999999999999556, 3.312500000000000000, -5.053300858899104853 ) ) ;
#681 = CARTESIAN_POINT ( 'NONE',  ( 7.773533131393477902, 4.718920071733073485, -20.62283890789821683 ) ) ;
#682 = CARTESIAN_POINT ( 'NONE',  ( 3.230086961373112242, 5.000000000003343992, 5.208283729180106292 ) ) ;
#683 = CIRCLE ( 'NONE', #6090, 1.000000000000000888 ) ;
#684 = CARTESIAN_POINT ( 'NONE',  ( 2.651650429449553759, 1.875000000000000000, -0.8483495705504471296 ) ) ;
#685 = APPROVAL_ROLE ( '' ) ;
#686 = CARTESIAN_POINT ( 'NONE',  ( 8.855022830454526428, 5.000000000000000888, -117.5519203246167876 ) ) ;
#687 = CARTESIAN_POINT ( 'NONE',  ( 0.000000000000000000, 4.000000000000000000, 0.000000000000000000 ) ) ;
#688 = VERTEX_POINT ( 'NONE', #88 ) ;
#689 = DIRECTION ( 'NONE',  ( 0.000000000000000000, 0.000000000000000000, 1.000000000000000000 ) ) ;
#690 = CARTESIAN_POINT ( 'NONE',  ( -2.298097038856279362, 3.875000000000000444, -5.798097038856278473 ) ) ;
#691 = CARTESIAN_POINT ( 'NONE',  ( -1.346194077712559167, 12.93750000000000178, -6.749999999999999112 ) ) ;
#692 = CARTESIAN_POINT ( 'NONE',  ( -17.32624372123753886, 2.500000000000000444, -131.8796757791585037 ) ) ;
#693 = CARTESIAN_POINT ( 'NONE',  ( 10.80856694317891176, 13.64261357360079074, -106.9774774610350789 ) ) ;
#694 = CARTESIAN_POINT ( 'NONE',  ( 3.249999999999999112, 6.812500000000000000, -2.153805922287439945 ) ) ;
#695 = CARTESIAN_POINT ( 'NONE',  ( -3.750000000000000000, 3.687500000000000444, -1.946699141100893149 ) ) ;
#696 = CARTESIAN_POINT ( 'NONE',  ( -3.750000000000000000, 10.25000000000000000, -3.499999999999999112 ) ) ;
#697 = LINE ( 'NONE', #14933, #4951 ) ;
#698 = VERTEX_POINT ( 'NONE', #7415 ) ;
#699 = CARTESIAN_POINT ( 'NONE',  ( -3.805953545085057677, 10.68988111647421846, -43.62564591857165652 ) ) ;
#700 = CARTESIAN_POINT ( 'NONE',  ( -4.592425496802573972E-16, 10.00000000000000000, -7.250000000000000000 ) ) ;
#701 = CARTESIAN_POINT ( 'NONE',  ( 8.475206276408092876, 0.000000000000000000, -34.56909192082981974 ) ) ;
#702 = DIRECTION ( 'NONE',  ( 0.000000000000000000, 0.000000000000000000, 1.000000000000000000 ) ) ;
#703 = DIRECTION ( 'NONE',  ( -0.9961255586397056438, 0.000000000000000000, 0.08794243244722428632 ) ) ;
#704 = ORIENTED_EDGE ( 'NONE', *, *, #7602, .F. ) ;
#705 = CARTESIAN_POINT ( 'NONE',  ( -26.83547194577748130, 4.000000000000714984, -174.1755862676965023 ) ) ;
#706 = CARTESIAN_POINT ( 'NONE',  ( 10.73855780921090641, 0.4779626745339241589, -164.7294754465163180 ) ) ;
#707 = CARTESIAN_POINT ( 'NONE',  ( -52.06782037834351939, 15.00000000000000000, -159.8510668928024359 ) ) ;
#708 = EDGE_CURVE ( 'NONE', #8297, #505, #6593, .T. ) ;
#709 = CARTESIAN_POINT ( 'NONE',  ( 2.651650429449552870, 14.12500000000000000, -6.151650429449555091 ) ) ;
#710 = ORIENTED_EDGE ( 'NONE', *, *, #5262, .F. ) ;
#711 = CARTESIAN_POINT ( 'NONE',  ( -14.68073284315481253, 7.499999999999991118, -92.37694453701993780 ) ) ;
#712 = CARTESIAN_POINT ( 'NONE',  ( -25.68053481550299111, -5.000000000000000888, -142.4798935003980773 ) ) ;
#713 = DIRECTION ( 'NONE',  ( -1.861571024194515387E-16, -1.000000000000000000, -2.108604941688510506E-15 ) ) ;
#714 = CARTESIAN_POINT ( 'NONE',  ( -20.63752471692298229, 8.673617379884034486E-16, -191.9478744570439233 ) ) ;
#715 = CARTESIAN_POINT ( 'NONE',  ( -1.346194077712559167, 8.937500000000000000, -6.749999999999999112 ) ) ;
#716 = DIRECTION ( 'NONE',  ( 0.8674617751425296452, 0.000000000000000000, 0.4975038378410473472 ) ) ;
#717 = CARTESIAN_POINT ( 'NONE',  ( -1.553300858899106629, -0.4374999999999998890, 0.2500000000000002220 ) ) ;
#718 = CARTESIAN_POINT ( 'NONE',  ( -14.68073284315481253, 7.499999999999991118, -92.37694453701993780 ) ) ;
#719 = VECTOR ( 'NONE', #9665, 1000.000000000000000 ) ;
#720 = CARTESIAN_POINT ( 'NONE',  ( 1.488703080326642114, 2.579293035051159144, -1.000000000000001332 ) ) ;
#721 = CARTESIAN_POINT ( 'NONE',  ( 1.346194077712558057, 11.56249999999999822, -6.750000000000000000 ) ) ;
#722 = CARTESIAN_POINT ( 'NONE',  ( 6.770579566034212071, 2.743867526398027223, -34.56909192082981974 ) ) ;
#723 = DIRECTION ( 'NONE',  ( 0.000000000000000000, 0.000000000000000000, -1.000000000000000000 ) ) ;
#724 = CARTESIAN_POINT ( 'NONE',  ( -1.346194077712559389, 8.437500000000000000, -6.749999999999999112 ) ) ;
#725 = CARTESIAN_POINT ( 'NONE',  ( 26.73765619226448464, 5.000000000000000888, -138.7442522361673127 ) ) ;
#726 = DIRECTION ( 'NONE',  ( -0.1564344650402312298, 0.000000000000000000, 0.9876883405951376593 ) ) ;
#727 = ORIENTED_EDGE ( 'NONE', *, *, #12802, .F. ) ;
#728 = EDGE_CURVE ( 'NONE', #8528, #2185, #3376, .T. ) ;
#729 = CARTESIAN_POINT ( 'NONE',  ( 10.97489471145172324, 5.773894329885068899, -44.95261283940258323 ) ) ;
#730 = CARTESIAN_POINT ( 'NONE',  ( -11.98491608995024649, 4.000000000000000888, -188.7215518410329196 ) ) ;
#731 = CARTESIAN_POINT ( 'NONE',  ( -2.651650429449553314, 1.375000000000000000, -6.151650429449552426 ) ) ;
#732 = CARTESIAN_POINT ( 'NONE',  ( 2.651650429449553314, 1.375000000000000000, -0.8483495705504476847 ) ) ;
#733 = EDGE_CURVE ( 'NONE', #7347, #6645, #12998, .T. ) ;
#734 = CARTESIAN_POINT ( 'NONE',  ( -3.980102097228897738E-16, 14.00000000000000000, -6.749999999999999112 ) ) ;
#735 = ORIENTED_EDGE ( 'NONE', *, *, #14546, .F. ) ;
#736 = CARTESIAN_POINT ( 'NONE',  ( -2.298097038856278473, 9.125000000000000000, -1.201902961143720416 ) ) ;
#737 = CARTESIAN_POINT ( 'NONE',  ( 10.00369055844187827, 12.49999999999999822, -46.08764602067113714 ) ) ;
#738 = CARTESIAN_POINT ( 'NONE',  ( -6.293558381461702211, 14.52912145056953719, -103.7844163225382772 ) ) ;
#739 = CARTESIAN_POINT ( 'NONE',  ( 4.275750346740477603, 0.3778493581961822056, 1.174871939900954620 ) ) ;
#740 = CARTESIAN_POINT ( 'NONE',  ( -9.513824166154529749, 11.41184093592985072, -116.4115394435323907 ) ) ;
#741 = COORDINATED_UNIVERSAL_TIME_OFFSET ( 0, 0, .AHEAD. ) ;
#742 = CARTESIAN_POINT ( 'NONE',  ( 8.317394296536116727, 12.49999999999999822, -114.4625571486762254 ) ) ;
#743 = FACE_OUTER_BOUND ( 'NONE', #171, .T. ) ;
#744 = CARTESIAN_POINT ( 'NONE',  ( 23.26395690036145680, 0.3310048020727625606, -138.4206416885019735 ) ) ;
#745 = VERTEX_POINT ( 'NONE', #1553 ) ;
#746 = CARTESIAN_POINT ( 'NONE',  ( 3.249999999999999112, 5.812500000000000000, -2.153805922287439945 ) ) ;
#747 = CARTESIAN_POINT ( 'NONE',  ( -29.69146998481285138, 4.000000000000000000, -183.7653926644912303 ) ) ;
#748 = CARTESIAN_POINT ( 'NONE',  ( -1.553300858899107073, 0.9375000000000002220, -7.249999999999999112 ) ) ;
#749 = EDGE_CURVE ( 'NONE', #14051, #14170, #2686, .T. ) ;
#750 = VERTEX_POINT ( 'NONE', #4948 ) ;
#751 = LOCAL_TIME ( 12, 28, 20.00000000000000000, #3676 ) ;
#752 = CARTESIAN_POINT ( 'NONE',  ( 3.800081604575823224, 1.749999999999317213, 48.85836690712316255 ) ) ;
#753 = CARTESIAN_POINT ( 'NONE',  ( 0.000000000000000000, 0.000000000000000000, -0.2500000000000002220 ) ) ;
#754 = AXIS2_PLACEMENT_3D ( 'NONE', #5135, #7448, #1582 ) ;
#755 = CARTESIAN_POINT ( 'NONE',  ( 2.651650429449553759, 6.875000000000000000, -0.8483495705504471296 ) ) ;
#756 = DIRECTION ( 'NONE',  ( -0.02181900108494696719, 0.000000000000000000, 0.9997619372588931741 ) ) ;
#757 = CARTESIAN_POINT ( 'NONE',  ( 0.03998412334521193878, 2.500000000000000888, 0.4529009045602684913 ) ) ;
#758 = CARTESIAN_POINT ( 'NONE',  ( 1.553300858899105963, 0.5625000000000002220, -7.250000000000000000 ) ) ;
#759 = DATE_AND_TIME ( #1916, #13072 ) ;
#760 = CARTESIAN_POINT ( 'NONE',  ( 2.298097038856278029, 13.12500000000000178, -5.798097038856279362 ) ) ;
#761 = CARTESIAN_POINT ( 'NONE',  ( -4.509114193367754986, 1.625551886426498394, -1.000000000000011768 ) ) ;
#762 = DIRECTION ( 'NONE',  ( 0.000000000000000000, 0.000000000000000000, -1.000000000000000000 ) ) ;
#763 = TOROIDAL_SURFACE ( 'NONE', #9394, 8.000000000000000000, 5.000000000000000000 ) ;
#764 = AXIS2_PLACEMENT_3D ( 'NONE', #12903, #2315, #4335 ) ;
#765 = ORIENTED_EDGE ( 'NONE', *, *, #6856, .T. ) ;
#766 = CARTESIAN_POINT ( 'NONE',  ( -68.96619529829705186, 10.00000000000000000, -201.1288088042396112 ) ) ;
#767 = CARTESIAN_POINT ( 'NONE',  ( 1.346194077712558279, 4.062500000000001776, -6.750000000000000888 ) ) ;
#768 = CARTESIAN_POINT ( 'NONE',  ( 30.96695154071790412, 8.773889247172311556, -44.17511166891541308 ) ) ;
#769 = CIRCLE ( 'NONE', #2753, 8.192786906463668473 ) ;
#770 = CARTESIAN_POINT ( 'NONE',  ( -9.302736714298539766, 4.336808689942017736E-16, -123.7731201990410597 ) ) ;
#771 = CIRCLE ( 'NONE', #11377, 6.000000000000005329 ) ;
#772 = CARTESIAN_POINT ( 'NONE',  ( 3.749999999999999556, 5.249999999999999112, -3.500000000000000444 ) ) ;
#773 = CIRCLE ( 'NONE', #6696, 0.5000000000000018874 ) ;
#774 = CARTESIAN_POINT ( 'NONE',  ( 3.749999999999999556, 8.812500000000000000, -1.946699141100892261 ) ) ;
#775 = CARTESIAN_POINT ( 'NONE',  ( 10.95001698349728336, 5.943472311793079221, -43.61737436169475046 ) ) ;
#776 = CARTESIAN_POINT ( 'NONE',  ( 3.890350893699055401, 0.000000000000000000, -1.782295516753907849 ) ) ;
#777 = CARTESIAN_POINT ( 'NONE',  ( -2.298097038856278918, 8.375000000000000000, -5.798097038856277585 ) ) ;
#778 = CARTESIAN_POINT ( 'NONE',  ( -3.749999999999999556, 10.75000000000000000, -3.499999999999999112 ) ) ;
#779 = FACE_OUTER_BOUND ( 'NONE', #3430, .T. ) ;
#780 = DIRECTION ( 'NONE',  ( 0.02181900108494707127, 0.000000000000000000, -0.9997619372588931741 ) ) ;
#781 = CARTESIAN_POINT ( 'NONE',  ( 9.049521024876144182, 0.9101575677978732681, -106.1719994250351533 ) ) ;
#782 = AXIS2_PLACEMENT_3D ( 'NONE', #7076, #13916, #9800 ) ;
#783 = ORIENTED_EDGE ( 'NONE', *, *, #6545, .F. ) ;
#784 = CARTESIAN_POINT ( 'NONE',  ( -27.95915014381559871, 4.000000000000232703, -177.3149405089903325 ) ) ;
#785 = DIRECTION ( 'NONE',  ( 0.08794243244722392550, 0.000000000000000000, 0.9961255586397055328 ) ) ;
#786 = CARTESIAN_POINT ( 'NONE',  ( -50.98844033420547106, 15.00000000000000000, -158.7499874894748757 ) ) ;
#787 = CARTESIAN_POINT ( 'NONE',  ( 2.298097038856278029, 4.125000000000000000, -5.798097038856279362 ) ) ;
#788 = VERTEX_POINT ( 'NONE', #3566 ) ;
#789 = DIRECTION ( 'NONE',  ( -0.000000000000000000, -1.000000000000000000, -0.000000000000000000 ) ) ;
#790 = CARTESIAN_POINT ( 'NONE',  ( 3.158384440324539355, 0.000000000000000000, -1.000000000000021760 ) ) ;
#791 = CYLINDRICAL_SURFACE ( 'NONE', #2074, 2.326940983401415419 ) ;
#792 = CARTESIAN_POINT ( 'NONE',  ( -49.26721305452312549, 5.000000000000000000, -156.1716796081737186 ) ) ;
#793 = CARTESIAN_POINT ( 'NONE',  ( 4.515869450397831386, 0.000000000000000000, -104.3391973869891416 ) ) ;
#794 = CARTESIAN_POINT ( 'NONE',  ( 1.346194077712561166, 8.437500000000000000, -0.2500000000000011102 ) ) ;
#795 = AXIS2_PLACEMENT_3D ( 'NONE', #13365, #1374, #6076 ) ;
#797 = EDGE_CURVE ( 'NONE', #6985, #13403, #11978, .T. ) ;
#796 = CARTESIAN_POINT ( 'NONE',  ( 1.123679064339592859, 4.590773665857039276, -139.4222662838609210 ) ) ;
#798 = CARTESIAN_POINT ( 'NONE',  ( -2.651650429449552870, 14.12500000000000000, -0.8483495705504462414 ) ) ;
#799 = CARTESIAN_POINT ( 'NONE',  ( -67.56077635250289859, 9.999999999999998224, -204.5805788406221097 ) ) ;
#800 = CARTESIAN_POINT ( 'NONE',  ( -8.141169791565570080, 12.70346812208739529, -105.1150889670498287 ) ) ;
#801 = EDGE_CURVE ( 'NONE', #750, #698, #14396, .T. ) ;
#802 = CARTESIAN_POINT ( 'NONE',  ( 0.000000000000000000, 12.00000000000000000, -0.2500000000000002220 ) ) ;
#803 = CARTESIAN_POINT ( 'NONE',  ( 4.529353718053122257, 2.743867526398027223, -43.69627513258503626 ) ) ;
#804 = CARTESIAN_POINT ( 'NONE',  ( -25.97807323962435078, -0.3396484172265533674, -142.5647913107548277 ) ) ;
#805 = CARTESIAN_POINT ( 'NONE',  ( 1.346194077712560944, 9.937499999999998224, -0.2500000000000010547 ) ) ;
#806 = CARTESIAN_POINT ( 'NONE',  ( 2.655454743645370375, 0.03267829224664529214, 0.8826354733248792384 ) ) ;
#807 = DIRECTION ( 'NONE',  ( 0.000000000000000000, -1.000000000000000000, 0.000000000000000000 ) ) ;
#808 = CC_DESIGN_APPROVAL ( #11527, ( #10180 ) ) ;
#809 = ORIENTED_EDGE ( 'NONE', *, *, #4890, .F. ) ;
#810 = CARTESIAN_POINT ( 'NONE',  ( -16.36917573835871309, 4.000000000000001776, -194.3843815398161894 ) ) ;
#811 = CARTESIAN_POINT ( 'NONE',  ( 1.553300858899105963, 15.06250000000000178, -7.249999999999999112 ) ) ;
#812 = CARTESIAN_POINT ( 'NONE',  ( 3.749999999999999112, 1.312500000000000000, -1.946699141100893149 ) ) ;
#813 = CARTESIAN_POINT ( 'NONE',  ( 3.249999999999999112, 1.812500000000000222, -2.153805922287439945 ) ) ;
#814 = VERTEX_POINT ( 'NONE', #6103 ) ;
#815 = CARTESIAN_POINT ( 'NONE',  ( 2.298097038856278473, 12.62500000000000000, -5.798097038856279362 ) ) ;
#816 = DIRECTION ( 'NONE',  ( 0.000000000000000000, 0.000000000000000000, -1.000000000000000000 ) ) ;
#817 = DIRECTION ( 'NONE',  ( 0.000000000000000000, -1.000000000000000000, 0.000000000000000000 ) ) ;
#818 = ADVANCED_FACE ( 'NONE', ( #233 ), #2402, .T. ) ;
#819 = CARTESIAN_POINT ( 'NONE',  ( -25.30358147364459143, 4.000000000000000000, -209.1611233605720201 ) ) ;
#820 = CARTESIAN_POINT ( 'NONE',  ( -9.030574454602195544, -2.490287375297125294, -34.97919997656152447 ) ) ;
#821 = CARTESIAN_POINT ( 'NONE',  ( 9.146012981469503700, 15.00000000000000000, -118.4481327387345857 ) ) ;
#822 = CYLINDRICAL_SURFACE ( 'NONE', #9374, 2.000000000000001776 ) ;
#823 = CARTESIAN_POINT ( 'NONE',  ( 1.243260443319662123, 4.179859613694246079, -139.4020581015306846 ) ) ;
#824 = ORIENTED_EDGE ( 'NONE', *, *, #13683, .T. ) ;
#825 = CARTESIAN_POINT ( 'NONE',  ( 1.346194077712558057, 3.562500000000000444, -6.750000000000000000 ) ) ;
#826 = CARTESIAN_POINT ( 'NONE',  ( -30.52456163227999753, 4.000000000000000000, -196.5486136056819362 ) ) ;
#827 = CARTESIAN_POINT ( 'NONE',  ( 3.749999999999999556, 0.2500000000000001110, -3.500000000000000444 ) ) ;
#828 = ORIENTED_EDGE ( 'NONE', *, *, #9715, .F. ) ;
#829 = CARTESIAN_POINT ( 'NONE',  ( 25.37742002255717466, 1.750000000000000000, 70.49803269364883818 ) ) ;
#830 = DIRECTION ( 'NONE',  ( 0.8645818496218652394, 0.000000000000000000, -0.5024920151648527566 ) ) ;
#831 = CARTESIAN_POINT ( 'NONE',  ( 3.749999999999998668, 4.687500000000000888, -5.053300858899107517 ) ) ;
#832 = CIRCLE ( 'NONE', #8231, 4.999999999999992895 ) ;
#833 = CARTESIAN_POINT ( 'NONE',  ( -25.67290302457112006, 1.351337947638526771, -206.3516727230842491 ) ) ;
#834 = EDGE_CURVE ( 'NONE', #5223, #6652, #7605, .T. ) ;
#835 = CARTESIAN_POINT ( 'NONE',  ( 0.2399920231728725206, 3.887405386441892485, 2.718394084632874463 ) ) ;
#836 = CARTESIAN_POINT ( 'NONE',  ( 3.749999999999999556, 2.812500000000000000, -1.946699141100892261 ) ) ;
#837 = EDGE_CURVE ( 'NONE', #10045, #8227, #6025, .T. ) ;
#838 = PERSON_AND_ORGANIZATION_ROLE ( 'design_owner' ) ;
#839 = EDGE_CURVE ( 'NONE', #4330, #9805, #4660, .T. ) ;
#840 = DIRECTION ( 'NONE',  ( 0.7575874476598363216, 0.000000000000000000, 0.6527336816407245390 ) ) ;
#841 = ORIENTED_EDGE ( 'NONE', *, *, #9714, .T. ) ;
#842 = CIRCLE ( 'NONE', #12440, 3.000000000000005329 ) ;
#843 = CC_DESIGN_DATE_AND_TIME_ASSIGNMENT ( #12095, #9626, ( #8846 ) ) ;
#844 = VECTOR ( 'NONE', #5757, 1000.000000000000000 ) ;
#845 = CARTESIAN_POINT ( 'NONE',  ( -3.249999999999999112, 1.687499999999999778, -2.153805922287440833 ) ) ;
#846 = CARTESIAN_POINT ( 'NONE',  ( 8.673617379884035472E-16, 15.00000000000000000, -1.663700395152567513 ) ) ;
#847 = CARTESIAN_POINT ( 'NONE',  ( -3.749999999999999556, 10.75000000000000178, -3.499999999999999112 ) ) ;
#848 = CARTESIAN_POINT ( 'NONE',  ( -4.592425496802573972E-16, 14.50000000000000000, -7.249999999999999112 ) ) ;
#849 = CARTESIAN_POINT ( 'NONE',  ( -8.817544209126905841, 2.675793395794448859, -115.6114935513795672 ) ) ;
#850 = CARTESIAN_POINT ( 'NONE',  ( -4.234402844927150689, 0.000000000000000000, -117.4888040839639558 ) ) ;
#851 = CARTESIAN_POINT ( 'NONE',  ( 3.249999999999998668, 7.687500000000000000, -4.846194077712560500 ) ) ;
#852 = CARTESIAN_POINT ( 'NONE',  ( 0.000000000000000000, 14.50000000000000000, 0.2500000000000002220 ) ) ;
#853 = CIRCLE ( 'NONE', #107, 1.000000000000000888 ) ;
#854 = DIRECTION ( 'NONE',  ( 0.000000000000000000, -0.000000000000000000, -1.000000000000000000 ) ) ;
#855 = APPROVAL_ROLE ( '' ) ;
#856 = CYLINDRICAL_SURFACE ( 'NONE', #10635, 3.500000000000000000 ) ;
#857 = CARTESIAN_POINT ( 'NONE',  ( 0.000000000000000000, 0.000000000000000000, -3.500000000000000000 ) ) ;
#858 = ORIENTED_EDGE ( 'NONE', *, *, #6268, .T. ) ;
#859 = CARTESIAN_POINT ( 'NONE',  ( -28.35615173165206215, 0.000000000000000000, -181.5209395138616912 ) ) ;
#860 = CARTESIAN_POINT ( 'NONE',  ( 1.052436484934206051, -2.529993217055220178, -1.000000000000021760 ) ) ;
#861 = CARTESIAN_POINT ( 'NONE',  ( -37.87309319206281089, 15.00000000000000000, -156.6288150090828424 ) ) ;
#862 = CARTESIAN_POINT ( 'NONE',  ( 1.346194077712561166, 4.437500000000001776, -0.2500000000000011102 ) ) ;
#863 = EDGE_LOOP ( 'NONE', ( #950, #5112, #7904, #11736 ) ) ;
#864 = CARTESIAN_POINT ( 'NONE',  ( -8.661991262811081782, 15.00000000000000000, -130.6821289911104600 ) ) ;
#865 = DIRECTION ( 'NONE',  ( 1.000000000000000000, 0.000000000000000000, 0.000000000000000000 ) ) ;
#866 = CARTESIAN_POINT ( 'NONE',  ( -25.59205555683100641, 2.114949368667459417, -207.6177744677006274 ) ) ;
#867 = CARTESIAN_POINT ( 'NONE',  ( 6.124315080327858318, 10.65467060482632178, 5.249130883299187644 ) ) ;
#868 = CARTESIAN_POINT ( 'NONE',  ( -1.499260709884682408, -1.623598343467119499E-12, -106.0110764664930940 ) ) ;
#869 = CARTESIAN_POINT ( 'NONE',  ( -1.346194077712558945, 11.56250000000000178, -0.2500000000000002220 ) ) ;
#870 = CARTESIAN_POINT ( 'NONE',  ( 22.05157068914783380, 5.000000000000000888, -147.3126055969165407 ) ) ;
#871 = CARTESIAN_POINT ( 'NONE',  ( 1.553300858899105963, 14.56250000000000000, -7.250000000000000888 ) ) ;
#872 = DIRECTION ( 'NONE',  ( -0.000000000000000000, -1.000000000000000000, -0.000000000000000000 ) ) ;
#873 = CARTESIAN_POINT ( 'NONE',  ( 1.831246893856137481, 2.490287375297123074, -1.000000000000007772 ) ) ;
#874 = PLANE ( 'NONE',  #5289 ) ;
#875 = CARTESIAN_POINT ( 'NONE',  ( -3.520407287333057855, 7.379999999999995453, -45.56125597433126018 ) ) ;
#876 = DIRECTION ( 'NONE',  ( -0.000000000000000000, -1.000000000000000000, -0.000000000000000000 ) ) ;
#877 = CARTESIAN_POINT ( 'NONE',  ( -2.298097038856278918, 7.375000000000000888, -5.798097038856277585 ) ) ;
#878 = CARTESIAN_POINT ( 'NONE',  ( 3.031377627837373634, 1.223715101037531339, 3.507052158993249069 ) ) ;
#879 = APPLICATION_CONTEXT ( 'configuration controlled 3d designs of mechanical parts and assemblies' ) ;
#880 = DIRECTION ( 'NONE',  ( -0.8674617751425297563, 0.000000000000000000, -0.4975038378410474027 ) ) ;
#881 = VERTEX_POINT ( 'NONE', #4261 ) ;
#882 = VERTEX_POINT ( 'NONE', #6343 ) ;
#883 = DIRECTION ( 'NONE',  ( 0.000000000000000000, 0.000000000000000000, 1.000000000000000000 ) ) ;
#884 = CARTESIAN_POINT ( 'NONE',  ( 3.749999999999999112, 2.812500000000000000, -1.946699141100892039 ) ) ;
#885 = CARTESIAN_POINT ( 'NONE',  ( 3.249999999999999556, 15.25000000000000355, -3.500000000000000000 ) ) ;
#886 = CARTESIAN_POINT ( 'NONE',  ( 30.50390178861119139, 1.750000000002257083, 35.39815044914973186 ) ) ;
#887 = VERTEX_POINT ( 'NONE', #474 ) ;
#888 = CARTESIAN_POINT ( 'NONE',  ( -3.249999999999999556, 7.250000000000000000, -3.499999999999999556 ) ) ;
#889 = CARTESIAN_POINT ( 'NONE',  ( 1.346194077712560944, 10.93750000000000000, -0.2500000000000010547 ) ) ;
#890 = CARTESIAN_POINT ( 'NONE',  ( 10.99170198404801724, 11.63674357114055624, -45.52741062780659576 ) ) ;
#891 = CARTESIAN_POINT ( 'NONE',  ( -8.398494254132010894, 12.74145370061613036, -104.4010416228292399 ) ) ;
#892 =( LENGTH_UNIT ( ) NAMED_UNIT ( * ) SI_UNIT ( .MILLI., .METRE. ) );
#893 = CARTESIAN_POINT ( 'NONE',  ( -9.817351912530863700, 10.77704051039747490, -115.7707972434356520 ) ) ;
#894 = COORDINATED_UNIVERSAL_TIME_OFFSET ( 0, 0, .AHEAD. ) ;
#895 = CARTESIAN_POINT ( 'NONE',  ( 7.666318370587849707, 15.00000000000000000, -107.4043470738708237 ) ) ;
#896 = CARTESIAN_POINT ( 'NONE',  ( -8.926802767664696603, 12.61830395633300661, -116.5496838980187988 ) ) ;
#897 = ORIENTED_EDGE ( 'NONE', *, *, #10097, .T. ) ;
#898 = CARTESIAN_POINT ( 'NONE',  ( 26.52981115270372925, 2.371853495815368973, -137.6347934788561247 ) ) ;
#899 = CARTESIAN_POINT ( 'NONE',  ( 3.249999999999998668, 11.68750000000000000, -4.846194077712560500 ) ) ;
#900 = ORIENTED_EDGE ( 'NONE', *, *, #13823, .F. ) ;
#901 = ORIENTED_EDGE ( 'NONE', *, *, #12261, .F. ) ;
#902 = CARTESIAN_POINT ( 'NONE',  ( 2.298097038856278473, 5.625000000000000000, -5.798097038856279362 ) ) ;
#903 = FACE_OUTER_BOUND ( 'NONE', #9111, .T. ) ;
#904 = CARTESIAN_POINT ( 'NONE',  ( 3.749999999999999556, 1.250000000000000222, -3.500000000000000444 ) ) ;
#905 = EDGE_LOOP ( 'NONE', ( #12470, #7304, #11009, #7164 ) ) ;
#906 = EDGE_CURVE ( 'NONE', #10778, #119, #6635, .T. ) ;
#907 = CARTESIAN_POINT ( 'NONE',  ( 0.5944212552585367293, 5.000000000000000888, -138.5540974747773930 ) ) ;
#908 = CARTESIAN_POINT ( 'NONE',  ( 1.346194077712560944, 0.9374999999999998890, -0.2500000000000010547 ) ) ;
#909 = CARTESIAN_POINT ( 'NONE',  ( 1.553300858899108849, 3.937500000000000000, 0.2499999999999993616 ) ) ;
#910 = CARTESIAN_POINT ( 'NONE',  ( 0.000000000000000000, 3.061616997868383018E-17, 0.2500000000000002220 ) ) ;
#911 = PERSON_AND_ORGANIZATION_ROLE ( 'design_supplier' ) ;
#912 = CARTESIAN_POINT ( 'NONE',  ( 10.23520164300409441, 4.999999999999998224, -120.8438954876117180 ) ) ;
#913 = DIRECTION ( 'NONE',  ( 0.9997619372588932851, 0.000000000000000000, 0.02181900108494707821 ) ) ;
#914 = VERTEX_POINT ( 'NONE', #12365 ) ;
#915 = CARTESIAN_POINT ( 'NONE',  ( 3.249999999999999556, 6.250000000000000000, -3.500000000000000000 ) ) ;
#916 = EDGE_CURVE ( 'NONE', #9927, #7124, #9915, .T. ) ;
#917 = DIRECTION ( 'NONE',  ( 0.9997619372588932851, 0.000000000000000000, 0.02181900108494707821 ) ) ;
#918 = ADVANCED_FACE ( 'NONE', ( #1933 ), #6818, .T. ) ;
#919 = CARTESIAN_POINT ( 'NONE',  ( -3.750000000000000000, 10.68750000000000178, -1.946699141100893149 ) ) ;
#920 = CARTESIAN_POINT ( 'NONE',  ( 2.651650429449553759, 11.87500000000000000, -0.8483495705504471296 ) ) ;
#921 = CARTESIAN_POINT ( 'NONE',  ( -66.05397366910187884, 15.01442789161885472, -199.5963413483335955 ) ) ;
#922 = VERTEX_POINT ( 'NONE', #7572 ) ;
#923 = CARTESIAN_POINT ( 'NONE',  ( -4.364759770003678874, -1.831210392890419758, -1.000000000000001332 ) ) ;
#924 = CARTESIAN_POINT ( 'NONE',  ( 3.249999999999999556, 7.750000000000000000, -3.500000000000000000 ) ) ;
#925 = CARTESIAN_POINT ( 'NONE',  ( 1.346194077712558279, 1.062500000000000444, -6.750000000000000888 ) ) ;
#926 = CARTESIAN_POINT ( 'NONE',  ( 11.05907272987663070, 13.62184257006102150, -106.3512328423712177 ) ) ;
#927 = CARTESIAN_POINT ( 'NONE',  ( -29.69515346086422980, 5.000000000000000000, -156.7390981038715836 ) ) ;
#928 = ORIENTED_EDGE ( 'NONE', *, *, #5981, .F. ) ;
#929 = CARTESIAN_POINT ( 'NONE',  ( -24.61704333935664124, 8.673617379884035472E-16, -200.7969854990674605 ) ) ;
#930 = CARTESIAN_POINT ( 'NONE',  ( -2.298097038856278918, 0.3750000000000000000, -5.798097038856277585 ) ) ;
#931 = CARTESIAN_POINT ( 'NONE',  ( -7.237223302401282865, 0.05734158322681513070, -104.4616748367153320 ) ) ;
#932 = CARTESIAN_POINT ( 'NONE',  ( 1.346194077712558279, 3.062500000000000000, -6.750000000000000888 ) ) ;
#933 = VERTEX_POINT ( 'NONE', #6415 ) ;
#934 = CYLINDRICAL_SURFACE ( 'NONE', #12406, 5.000000000000000000 ) ;
#935 = EDGE_CURVE ( 'NONE', #7022, #7777, #15292, .T. ) ;
#936 = CARTESIAN_POINT ( 'NONE',  ( -3.942526376314868131, 15.00000000000000178, -136.1336533158788029 ) ) ;
#937 = CARTESIAN_POINT ( 'NONE',  ( 8.954400122595130185, 11.89263850632991293, 1.991577900038186799 ) ) ;
#938 = CARTESIAN_POINT ( 'NONE',  ( -4.781971238309704830, 1.734723475976807094E-15, -110.8602639898849418 ) ) ;
#939 = CARTESIAN_POINT ( 'NONE',  ( -2.298097038856278029, 10.62500000000000178, -1.201902961143720638 ) ) ;
#940 = CARTESIAN_POINT ( 'NONE',  ( -25.82983890416511841, 9.999999999999998224, -142.4527639562402328 ) ) ;
#941 = CARTESIAN_POINT ( 'NONE',  ( -3.750000000000000000, 1.812499999999999778, -5.053300858899105741 ) ) ;
#942 = CARTESIAN_POINT ( 'NONE',  ( 0.5065669489466559927, 9.999999999999998224, 5.737893198614714585 ) ) ;
#943 = CARTESIAN_POINT ( 'NONE',  ( 1.170341033097332506, 2.410101856083639138, -1.000000000000001110 ) ) ;
#944 = DIRECTION ( 'NONE',  ( 0.000000000000000000, 0.000000000000000000, 1.000000000000000000 ) ) ;
#945 = CARTESIAN_POINT ( 'NONE',  ( 3.586150740732019226, 2.099999999999147438, 48.99645249886114584 ) ) ;
#946 = CARTESIAN_POINT ( 'NONE',  ( -3.249999999999999556, 10.25000000000000000, -3.499999999999999556 ) ) ;
#947 = CARTESIAN_POINT ( 'NONE',  ( -1.437999228988334544, 5.000000000000000888, -140.6782968106692522 ) ) ;
#948 = CARTESIAN_POINT ( 'NONE',  ( 26.30339064689345463, 0.000000000000000000, 68.98786334397659914 ) ) ;
#949 = ORIENTED_EDGE ( 'NONE', *, *, #8090, .T. ) ;
#950 = ORIENTED_EDGE ( 'NONE', *, *, #9967, .F. ) ;
#951 = CARTESIAN_POINT ( 'NONE',  ( 0.1414445318493903758, 0.000000000000000000, -169.8395012284044867 ) ) ;
#952 = CARTESIAN_POINT ( 'NONE',  ( 3.749999999999999556, 15.25000000000000355, -3.500000000000000444 ) ) ;
#953 = CARTESIAN_POINT ( 'NONE',  ( 3.249999999999998224, 13.31250000000000178, -2.153805922287439945 ) ) ;
#954 = CARTESIAN_POINT ( 'NONE',  ( 26.64925767285982161, 4.000000000000000000, -138.6957041034480653 ) ) ;
#955 = EDGE_LOOP ( 'NONE', ( #6140, #13422, #2165, #11339 ) ) ;
#956 = CARTESIAN_POINT ( 'NONE',  ( -1.346194077712559389, 14.43750000000000000, -6.749999999999999112 ) ) ;
#957 = CARTESIAN_POINT ( 'NONE',  ( 0.000000000000000000, 5.000000000000000888, -100.6237003951525679 ) ) ;
#958 = CARTESIAN_POINT ( 'NONE',  ( 46.59046791724578895, 0.000000000000000000, 61.03149078395468763 ) ) ;
#959 = CARTESIAN_POINT ( 'NONE',  ( -1.346194077712559389, 5.437500000000002665, -6.749999999999999112 ) ) ;
#960 = COORDINATED_UNIVERSAL_TIME_OFFSET ( 0, 0, .AHEAD. ) ;
#961 = CARTESIAN_POINT ( 'NONE',  ( 9.667889503803975160, 12.49999999999999822, -108.9228968456644537 ) ) ;
#962 = CARTESIAN_POINT ( 'NONE',  ( 4.286263797015736595E-16, 1.000000000000000000, 3.500000000000000000 ) ) ;
#963 = ORIENTED_EDGE ( 'NONE', *, *, #9785, .F. ) ;
#964 = B_SPLINE_CURVE_WITH_KNOTS ( 'NONE', 3,
 ( #5074, #8538, #4909, #11858, #14518, #2441, #7135, #1283, #10709, #9624, #4837, #14357, #9549, #14275, #7376, #3756 ),
 .UNSPECIFIED., .F., .F.,
 ( 4, 2, 2, 2, 2, 2, 2, 4 ),
 ( -1.886156721772299085E-05, 0.0008578064990923553543, 0.001734474565402433811, 0.003487810698022590292, 0.004364478764332667231, 0.005241146830642744170, 0.006117814896952821109, 0.006994482963262898048 ),
 .UNSPECIFIED. ) ;
#965 = CARTESIAN_POINT ( 'NONE',  ( 26.98129511509239720, 4.223198481478519284, -138.2263353510321053 ) ) ;
#966 = CARTESIAN_POINT ( 'NONE',  ( 2.298097038856279362, 11.87500000000000000, -1.201902961143720860 ) ) ;
#967 = EDGE_LOOP ( 'NONE', ( #8072, #15134, #4528, #327 ) ) ;
#968 = EDGE_LOOP ( 'NONE', ( #12812, #2857, #5859, #13093 ) ) ;
#969 = CARTESIAN_POINT ( 'NONE',  ( 1.553300858899105963, 9.062500000000000000, -7.250000000000000888 ) ) ;
#970 = CARTESIAN_POINT ( 'NONE',  ( -20.64382723625413263, 3.999999999999999112, -161.8400422034196424 ) ) ;
#971 = CARTESIAN_POINT ( 'NONE',  ( -3.750000000000000000, 0.8125000000000001110, -5.053300858899105741 ) ) ;
#972 = CARTESIAN_POINT ( 'NONE',  ( 1.346194077712561166, 5.437500000000000888, -0.2500000000000011102 ) ) ;
#973 = VERTEX_POINT ( 'NONE', #13693 ) ;
#974 = CARTESIAN_POINT ( 'NONE',  ( 1.893911505664648054, 5.000000000000000888, -1.663006917529762152 ) ) ;
#975 = CARTESIAN_POINT ( 'NONE',  ( -2.298097038856278918, 4.375000000000000000, -5.798097038856277585 ) ) ;
#976 = CARTESIAN_POINT ( 'NONE',  ( -2.651650429449552870, 7.125000000000000000, -0.8483495705504462414 ) ) ;
#977 = CARTESIAN_POINT ( 'NONE',  ( -25.49856690235932177, 3.011500147457180976, -208.5102016022315752 ) ) ;
#978 = CARTESIAN_POINT ( 'NONE',  ( -0.4453226528549816265, -2.225540348348185052E-17, -1.000000000000000000 ) ) ;
#979 = EDGE_CURVE ( 'NONE', #2743, #333, #11479, .T. ) ;
#980 = DATE_AND_TIME ( #6851, #3448 ) ;
#981 = EDGE_CURVE ( 'NONE', #10451, #3740, #9627, .T. ) ;
#982 = CARTESIAN_POINT ( 'NONE',  ( 14.55113584266641169, 5.000000000000001776, -126.9185724433401248 ) ) ;
#983 = CC_DESIGN_SECURITY_CLASSIFICATION ( #9370, ( #12333 ) ) ;
#984 = ORIENTED_EDGE ( 'NONE', *, *, #4488, .T. ) ;
#985 = CONICAL_SURFACE ( 'NONE', #15311, 0.5000000000000004441, 0.6283185307179600665 ) ;
#986 = CARTESIAN_POINT ( 'NONE',  ( 1.346194077712561166, 6.437499999999999112, -0.2500000000000011102 ) ) ;
#987 = CARTESIAN_POINT ( 'NONE',  ( -3.664341105599659976, 9.999999999999994671, -109.4598404583043987 ) ) ;
#988 = CARTESIAN_POINT ( 'NONE',  ( -2.651650429449552870, 7.874999999999999112, -6.151650429449552426 ) ) ;
#989 = CARTESIAN_POINT ( 'NONE',  ( 1.553300858899108849, 11.93750000000000000, 0.2499999999999993616 ) ) ;
#990 = LOCAL_TIME ( 12, 28, 20.00000000000000000, #14421 ) ;
#991 = CARTESIAN_POINT ( 'NONE',  ( -14.85661770804926007, 7.499999999999991118, -94.36919565429934664 ) ) ;
#992 = CARTESIAN_POINT ( 'NONE',  ( 4.999999999999998224, 0.000000000000000000, -45.97309604003007877 ) ) ;
#993 = CARTESIAN_POINT ( 'NONE',  ( -3.750000000000000000, 13.68750000000000178, -1.946699141100893149 ) ) ;
#994 = CARTESIAN_POINT ( 'NONE',  ( -2.958380929922356906, 4.336808689942018722E-16, -110.3652039456601983 ) ) ;
#995 = CIRCLE ( 'NONE', #12103, 5.000000000000000000 ) ;
#996 = APPROVAL_ROLE ( '' ) ;
#997 = EDGE_CURVE ( 'NONE', #7124, #9927, #12825, .T. ) ;
#998 = CARTESIAN_POINT ( 'NONE',  ( 0.000000000000000000, 1.000000000000000000, 0.000000000000000000 ) ) ;
#999 = ORIENTED_EDGE ( 'NONE', *, *, #11506, .T. ) ;
#1000 = DIRECTION ( 'NONE',  ( 0.7575874476598360996, -0.000000000000000000, 0.6527336816407247611 ) ) ;
#1001 = CARTESIAN_POINT ( 'NONE',  ( -3.249999999999999556, 4.250000000000000000, -3.499999999999999556 ) ) ;
#1002 = CARTESIAN_POINT ( 'NONE',  ( -56.34877470247857900, 15.00000000000000000, -165.2605511895863799 ) ) ;
#1003 = TOROIDAL_SURFACE ( 'NONE', #9148, 2.000000000000000000, 5.000000000000000000 ) ;
#1004 = CARTESIAN_POINT ( 'NONE',  ( -2.298097038856279362, 3.875000000000000444, -5.798097038856278473 ) ) ;
#1005 = ORIENTED_EDGE ( 'NONE', *, *, #13682, .T. ) ;
#1006 = DIRECTION ( 'NONE',  ( 0.000000000000000000, 0.000000000000000000, -1.000000000000000000 ) ) ;
#1007 =( BOUNDED_CURVE ( )  B_SPLINE_CURVE ( 3, ( #8686, #2825, #4208, #6294 ),
 .UNSPECIFIED., .F., .T. ) 
 B_SPLINE_CURVE_WITH_KNOTS ( ( 4, 4 ),
 ( 4.517782591535512537, 4.712388980384686121 ),
 .UNSPECIFIED. ) 
 CURVE ( )  GEOMETRIC_REPRESENTATION_ITEM ( )  RATIONAL_B_SPLINE_CURVE ( ( 1.000000000000000000, 0.9968465187034001307, 0.9968465187034001307, 1.000000000000000000 ) ) 
 REPRESENTATION_ITEM ( '' )  );
#1008 = CARTESIAN_POINT ( 'NONE',  ( 6.288457687488933523, 0.000000000000000000, -105.0111312234435985 ) ) ;
#1009 = AXIS2_PLACEMENT_3D ( 'NONE', #1918, #12811, #762 ) ;
#1010 = DIRECTION ( 'NONE',  ( 0.000000000000000000, 1.000000000000000000, 0.000000000000000000 ) ) ;
#1011 = CARTESIAN_POINT ( 'NONE',  ( -1.334601435215332810, 5.000000000000000888, -105.6792246796211572 ) ) ;
#1012 = CARTESIAN_POINT ( 'NONE',  ( -3.249999999999999556, 11.75000000000000178, -3.500000000000000000 ) ) ;
#1013 = CC_DESIGN_DATE_AND_TIME_ASSIGNMENT ( #2353, #2048, ( #9134 ) ) ;
#1014 = CARTESIAN_POINT ( 'NONE',  ( 13.15367060044211733, 5.000000000000000888, -166.3809663071982641 ) ) ;
#1015 = CARTESIAN_POINT ( 'NONE',  ( 2.651650429449554203, 0.3750000000000001110, -0.8483495705504471296 ) ) ;
#1016 = FACE_OUTER_BOUND ( 'NONE', #12058, .T. ) ;
#1017 = AXIS2_PLACEMENT_3D ( 'NONE', #10308, #11372, #6808 ) ;
#1018 = CARTESIAN_POINT ( 'NONE',  ( 1.077441151898745231, 2.255542499959171554, -1.000000000000001776 ) ) ;
#1019 = EDGE_CURVE ( 'NONE', #8185, #8798, #11512, .T. ) ;
#1020 = EDGE_CURVE ( 'NONE', #2289, #4876, #7951, .T. ) ;
#1021 = CARTESIAN_POINT ( 'NONE',  ( -7.773700879994175139, 9.999999999999998224, -121.5245725921722908 ) ) ;
#1022 = EDGE_CURVE ( 'NONE', #9480, #7043, #3333, .T. ) ;
#1023 = CARTESIAN_POINT ( 'NONE',  ( -5.011228476432583179, 0.000000000000000000, 8.417957015065626436 ) ) ;
#1024 = CARTESIAN_POINT ( 'NONE',  ( 0.000000000000000000, 10.00000000000000000, -0.2500000000000002220 ) ) ;
#1025 = DIRECTION ( 'NONE',  ( 1.000000000000000000, 0.000000000000000000, 0.000000000000000000 ) ) ;
#1026 = CARTESIAN_POINT ( 'NONE',  ( 0.000000000000000000, 3.061616997868383018E-17, 0.1491815183709511716 ) ) ;
#1027 = VERTEX_POINT ( 'NONE', #857 ) ;
#1028 = ORIENTED_EDGE ( 'NONE', *, *, #10486, .T. ) ;
#1029 = CARTESIAN_POINT ( 'NONE',  ( -15.99371261050736059, 8.673617379884035472E-16, -185.9135522072651270 ) ) ;
#1030 = CARTESIAN_POINT ( 'NONE',  ( -2.651650429449553314, 5.375000000000000000, -6.151650429449552426 ) ) ;
#1031 = CARTESIAN_POINT ( 'NONE',  ( -2.651650429449552870, 1.625000000000000000, -0.8483495705504467965 ) ) ;
#1032 = FACE_OUTER_BOUND ( 'NONE', #11557, .T. ) ;
#1033 = ORIENTED_EDGE ( 'NONE', *, *, #162, .F. ) ;
#1034 = AXIS2_PLACEMENT_3D ( 'NONE', #978, #50, #11786 ) ;
#1035 = CARTESIAN_POINT ( 'NONE',  ( -3.249999999999999556, 13.25000000000000000, -3.499999999999999556 ) ) ;
#1036 = PLANE ( 'NONE',  #13106 ) ;
#1037 = DIRECTION ( 'NONE',  ( 0.9982196940171963462, 0.000000000000000000, -0.05964429961207440289 ) ) ;
#1038 = CARTESIAN_POINT ( 'NONE',  ( 3.249999999999999556, 2.750000000000000000, -3.500000000000000000 ) ) ;
#1039 = DATE_TIME_ROLE ( 'classification_date' ) ;
#1040 = LOCAL_TIME ( 12, 28, 20.00000000000000000, #10425 ) ;
#1041 = CARTESIAN_POINT ( 'NONE',  ( 8.122171302341582688, 15.00000000000000000, -106.7308232591198447 ) ) ;
#1042 = PLANE ( 'NONE',  #8379 ) ;
#1043 = VERTEX_POINT ( 'NONE', #927 ) ;
#1044 = CARTESIAN_POINT ( 'NONE',  ( -3.231884997086563516, 15.00000000000000178, -104.1825805049879108 ) ) ;
#1045 = CARTESIAN_POINT ( 'NONE',  ( 1.346194077712560944, 12.93750000000000355, -0.2500000000000011102 ) ) ;
#1046 = PRODUCT_DEFINITION ( 'UNKNOWN', '', #10666, #4186 ) ;
#1047 = ORIENTED_EDGE ( 'NONE', *, *, #3849, .F. ) ;
#1048 = ORIENTED_EDGE ( 'NONE', *, *, #1468, .F. ) ;
#1049 = CARTESIAN_POINT ( 'NONE',  ( 3.750000000000000000, 8.312500000000003553, -1.946699141100892705 ) ) ;
#1050 = CARTESIAN_POINT ( 'NONE',  ( 8.990525241558630754, 12.49999999999999822, 0.3362996048474836686 ) ) ;
#1051 = CARTESIAN_POINT ( 'NONE',  ( -1.553300858899107073, 6.937500000000001776, -7.249999999999999112 ) ) ;
#1052 = CARTESIAN_POINT ( 'NONE',  ( 3.249999999999998224, 6.312500000000000000, -2.153805922287439945 ) ) ;
#1053 = EDGE_LOOP ( 'NONE', ( #12778, #8600, #2407, #11031 ) ) ;
#1054 = CARTESIAN_POINT ( 'NONE',  ( 2.958795351717913302, 15.00000000000000000, -108.2770199283341270 ) ) ;
#1055 = CARTESIAN_POINT ( 'NONE',  ( -3.249999999999999556, 3.187500000000000000, -2.153805922287440833 ) ) ;
#1056 = LOCAL_TIME ( 12, 28, 20.00000000000000000, #7554 ) ;
#1057 = CARTESIAN_POINT ( 'NONE',  ( 3.750000000000000000, 7.750000000000000000, -3.500000000000000444 ) ) ;
#1058 = CARTESIAN_POINT ( 'NONE',  ( -25.69488127297490010, 1.053316850392583603, -205.6773358527060509 ) ) ;
#1059 = DIRECTION ( 'NONE',  ( 0.000000000000000000, 0.000000000000000000, -1.000000000000000000 ) ) ;
#1060 = AXIS2_PLACEMENT_3D ( 'NONE', #711, #5115, #2802 ) ;
#1061 = APPROVAL_DATE_TIME ( #980, #10017 ) ;
#1062 = LINE ( 'NONE', #4616, #7254 ) ;
#1063 = VERTEX_POINT ( 'NONE', #10505 ) ;
#1064 = CARTESIAN_POINT ( 'NONE',  ( -2.298097038856278029, 7.625000000000000000, -1.201902961143720638 ) ) ;
#1065 = EDGE_CURVE ( 'NONE', #4658, #6698, #2103, .T. ) ;
#1066 = CARTESIAN_POINT ( 'NONE',  ( 8.475206276408092876, 1.020558061026469510, -34.56909192082981974 ) ) ;
#1067 = VECTOR ( 'NONE', #3211, 1000.000000000000000 ) ;
#1068 = CARTESIAN_POINT ( 'NONE',  ( 0.000000000000000000, 7.499999999999999112, 0.2499999999999998057 ) ) ;
#1069 = CARTESIAN_POINT ( 'NONE',  ( 10.94790802041947941, 11.56847231179307656, -43.52074019388548010 ) ) ;
#1070 = CARTESIAN_POINT ( 'NONE',  ( -67.52238797519952129, 13.85924130086240602, -199.4941995012791267 ) ) ;
#1071 = CARTESIAN_POINT ( 'NONE',  ( -1.655958715138094783, 0.9295642660359961784, -137.9252659957873561 ) ) ;
#1072 = CARTESIAN_POINT ( 'NONE',  ( 3.249999999999999112, 7.812500000000000000, -2.153805922287439945 ) ) ;
#1073 = CARTESIAN_POINT ( 'NONE',  ( -3.750000000000000000, 13.81250000000000178, -5.053300858899105741 ) ) ;
#1074 = CARTESIAN_POINT ( 'NONE',  ( 5.844703153020811115, 9.999999999999998224, -103.2023327213425432 ) ) ;
#1075 = PERSON_AND_ORGANIZATION_ROLE ( 'creator' ) ;
#1076 = CIRCLE ( 'NONE', #9720, 3.000000000000005329 ) ;
#1077 = CARTESIAN_POINT ( 'NONE',  ( 9.978237861888676008, 4.811578193488561084, -45.08415836920456599 ) ) ;
#1078 = AXIS2_PLACEMENT_3D ( 'NONE', #10444, #9206, #15103 ) ;
#1079 = VERTEX_POINT ( 'NONE', #5708 ) ;
#1080 = CARTESIAN_POINT ( 'NONE',  ( -30.01749617214946042, 3.999999999999751754, -199.5820917270032453 ) ) ;
#1081 = CARTESIAN_POINT ( 'NONE',  ( 3.249999999999999556, 4.750000000000000000, -3.500000000000000000 ) ) ;
#1082 = CARTESIAN_POINT ( 'NONE',  ( -61.70104298252753949, 14.99999999999465849, -192.5140885290328185 ) ) ;
#1083 = CARTESIAN_POINT ( 'NONE',  ( -1.346194077712559167, 0.9375000000000002220, -6.749999999999999112 ) ) ;
#1084 = ORIENTED_EDGE ( 'NONE', *, *, #2239, .T. ) ;
#1085 = CARTESIAN_POINT ( 'NONE',  ( 46.59046791724578895, 1.632027846198980036E-15, 61.03149078395468763 ) ) ;
#1086 = DIRECTION ( 'NONE',  ( 1.000000000000000000, 0.000000000000000000, 0.000000000000000000 ) ) ;
#1087 = CARTESIAN_POINT ( 'NONE',  ( 8.938384216414224426, 10.81018948157493220, 2.725437957519308618 ) ) ;
#1088 = EDGE_CURVE ( 'NONE', #1352, #13049, #14712, .T. ) ;
#1089 = CARTESIAN_POINT ( 'NONE',  ( -8.289881740238502772, -2.075239479414269894, -35.21986562831451550 ) ) ;
#1090 = CARTESIAN_POINT ( 'NONE',  ( 3.249999999999999556, 13.25000000000000178, -3.500000000000000000 ) ) ;
#1091 = AXIS2_PLACEMENT_3D ( 'NONE', #4040, #8970, #8745 ) ;
#1092 = CARTESIAN_POINT ( 'NONE',  ( 4.999999999999999112, 0.000000000000000000, -100.6237003951525679 ) ) ;
#1093 = CARTESIAN_POINT ( 'NONE',  ( 2.651650429449552870, 1.124999999999999778, -6.151650429449555091 ) ) ;
#1094 = CARTESIAN_POINT ( 'NONE',  ( -1.500000000000000000, 4.500000000000000888, -0.2499999999999997780 ) ) ;
#1095 = CARTESIAN_POINT ( 'NONE',  ( -0.3766621274091715987, 0.5000000000000000000, 0.1491815183709511716 ) ) ;
#1096 = CARTESIAN_POINT ( 'NONE',  ( -5.795830733078562780, 9.999999999999998224, -117.2993747367960253 ) ) ;
#1097 = CARTESIAN_POINT ( 'NONE',  ( -7.119039342394801295, 2.100000000000745715, 20.68784477908849340 ) ) ;
#1098 = CARTESIAN_POINT ( 'NONE',  ( -3.249999999999999556, 14.31250000000000000, -4.846194077712557835 ) ) ;
#1099 = AXIS2_PLACEMENT_3D ( 'NONE', #8541, #6456, #8617 ) ;
#1100 = DIRECTION ( 'NONE',  ( 0.000000000000000000, 0.000000000000000000, -1.000000000000000000 ) ) ;
#1101 = CARTESIAN_POINT ( 'NONE',  ( 27.03835354040193195, 5.000000000000000888, -138.2189567750509980 ) ) ;
#1102 = ORIENTED_EDGE ( 'NONE', *, *, #11420, .T. ) ;
#1103 = B_SPLINE_CURVE_WITH_KNOTS ( 'NONE', 3,
 ( #3789, #14551, #10897, #9819, #470, #7410, #6410, #14391, #11129, #13230, #2869, #3947, #7568, #8572, #5183, #9578 ),
 .UNSPECIFIED., .F., .F.,
 ( 4, 2, 2, 2, 2, 2, 2, 4 ),
 ( 0.000000000000000000, 0.0004969249972743298906, 0.0009938499945486597813, 0.001490774991822989672, 0.001987699989097319563, 0.002981549983645979344, 0.003478474980920309018, 0.003975399978194639125 ),
 .UNSPECIFIED. ) ;
#1104 = ORIENTED_EDGE ( 'NONE', *, *, #2330, .T. ) ;
#1105 = DIRECTION ( 'NONE',  ( 0.000000000000000000, -1.000000000000000000, 0.000000000000000000 ) ) ;
#1106 = CARTESIAN_POINT ( 'NONE',  ( 1.553300858899108849, 4.937500000000001776, 0.2499999999999993616 ) ) ;
#1107 = CARTESIAN_POINT ( 'NONE',  ( -3.750000000000000000, 2.812500000000000444, -5.053300858899105741 ) ) ;
#1108 = CARTESIAN_POINT ( 'NONE',  ( 5.079523875978591896, 15.00000000000802558, -108.2552591983019994 ) ) ;
#1109 = ORIENTED_EDGE ( 'NONE', *, *, #2808, .T. ) ;
#1110 = EDGE_CURVE ( 'NONE', #10252, #14298, #4559, .T. ) ;
#1111 = CARTESIAN_POINT ( 'NONE',  ( 2.298097038856278473, 13.62500000000000000, -5.798097038856279362 ) ) ;
#1112 = EDGE_CURVE ( 'NONE', #5602, #8895, #4401, .T. ) ;
#1113 = EDGE_CURVE ( 'NONE', #9776, #13724, #15007, .T. ) ;
#1114 = DIRECTION ( 'NONE',  ( 0.000000000000000000, 1.000000000000000000, 0.000000000000000000 ) ) ;
#1115 = CARTESIAN_POINT ( 'NONE',  ( 39.66138262230233380, 2.099999999999999645, 42.07085476361616116 ) ) ;
#1116 = CARTESIAN_POINT ( 'NONE',  ( -2.298097038856278918, 5.375000000000000000, -5.798097038856277585 ) ) ;
#1117 = ITEM_DEFINED_TRANSFORMATION ( 'NONE', 'NONE', #15127,  #9419 ) ;
#1118 = CYLINDRICAL_SURFACE ( 'NONE', #9743, 1.000000000000000888 ) ;
#1119 = CARTESIAN_POINT ( 'NONE',  ( 18.61385351463323090, 8.673617379884035472E-16, -137.3217374087719520 ) ) ;
#1120 = VERTEX_POINT ( 'NONE', #13992 ) ;
#1121 = CARTESIAN_POINT ( 'NONE',  ( 2.035195838443857763, -2.353283696435568118, -1.000000000000001110 ) ) ;
#1122 = CARTESIAN_POINT ( 'NONE',  ( 2.298097038856279362, 12.87500000000000178, -1.201902961143720860 ) ) ;
#1123 = ORIENTED_EDGE ( 'NONE', *, *, #12013, .T. ) ;
#1124 = VERTEX_POINT ( 'NONE', #7016 ) ;
#1125 = CARTESIAN_POINT ( 'NONE',  ( -9.721966606378851239, 10.00000000000000000, -116.3614657639809309 ) ) ;
#1126 = CARTESIAN_POINT ( 'NONE',  ( 3.749999999999999556, 7.250000000000001776, -3.500000000000000444 ) ) ;
#1127 = CARTESIAN_POINT ( 'NONE',  ( 2.298097038856279362, 6.375000000000000888, -1.201902961143720860 ) ) ;
#1128 = ORIENTED_EDGE ( 'NONE', *, *, #2993, .F. ) ;
#1129 = CARTESIAN_POINT ( 'NONE',  ( 0.2132689653709242128, 15.00000000000000000, -112.6263465441548561 ) ) ;
#1130 = CARTESIAN_POINT ( 'NONE',  ( 1.346194077712560944, 3.937500000000000000, -0.2500000000000010547 ) ) ;
#1131 = ADVANCED_FACE ( 'NONE', ( #1150, #5628 ), #10343, .T. ) ;
#1132 = CARTESIAN_POINT ( 'NONE',  ( 2.651650429449553759, 9.875000000000000000, -0.8483495705504471296 ) ) ;
#1133 = B_SPLINE_CURVE_WITH_KNOTS ( 'NONE', 3,
 ( #10230, #10373, #725, #4427 ),
 .UNSPECIFIED., .F., .F.,
 ( 4, 4 ),
 ( 0.000000000000000000, 0.0009078663748908937306 ),
 .UNSPECIFIED. ) ;
#1134 = CARTESIAN_POINT ( 'NONE',  ( -24.64352728812290039, 3.658198090794281931, -208.7829853464023984 ) ) ;
#1135 = DIRECTION ( 'NONE',  ( 0.000000000000000000, 0.000000000000000000, -1.000000000000000000 ) ) ;
#1136 = DIRECTION ( 'NONE',  ( 0.000000000000000000, 1.000000000000000000, 0.000000000000000000 ) ) ;
#1137 = SHAPE_DEFINITION_REPRESENTATION ( #3882, #9812 ) ;
#1138 = DIRECTION ( 'NONE',  ( 0.000000000000000000, -1.000000000000000000, 0.000000000000000000 ) ) ;
#1139 = ORIENTED_EDGE ( 'NONE', *, *, #7503, .F. ) ;
#1140 = CARTESIAN_POINT ( 'NONE',  ( -3.249999999999999112, 7.687500000000000000, -2.153805922287440833 ) ) ;
#1141 = CARTESIAN_POINT ( 'NONE',  ( -0.8336906130587268260, 1.921202954650395700, -45.08225561976306039 ) ) ;
#1142 = CARTESIAN_POINT ( 'NONE',  ( -2.651650429449552870, 9.875000000000000000, -6.151650429449552426 ) ) ;
#1143 = CARTESIAN_POINT ( 'NONE',  ( 52.73038795364751508, 1.750000000000000000, 69.25342193720584305 ) ) ;
#1144 = CARTESIAN_POINT ( 'NONE',  ( -65.74075837058826721, 15.17285174006052273, -202.4370987171274408 ) ) ;
#1145 = CARTESIAN_POINT ( 'NONE',  ( -4.975935430107378821, 0.000000000000000000, -1.000000000000001332 ) ) ;
#1146 = CARTESIAN_POINT ( 'NONE',  ( 1.346194077712561166, 0.4375000000000000555, -0.2500000000000011102 ) ) ;
#1147 = PLANE ( 'NONE',  #7230 ) ;
#1148 = APPROVAL_STATUS ( 'not_yet_approved' ) ;
#1149 = CARTESIAN_POINT ( 'NONE',  ( -3.980102097228897245E-16, 14.50000000000000000, -6.749999999999999112 ) ) ;
#1150 = FACE_OUTER_BOUND ( 'NONE', #11865, .T. ) ;
#1151 = EDGE_LOOP ( 'NONE', ( #10949, #5671, #3319 ) ) ;
#1152 = CARTESIAN_POINT ( 'NONE',  ( -22.03984370847868490, 0.000000000000000000, -205.5299584989701600 ) ) ;
#1153 = CARTESIAN_POINT ( 'NONE',  ( -2.298097038856278473, 4.125000000000000000, -1.201902961143720416 ) ) ;
#1154 = CARTESIAN_POINT ( 'NONE',  ( -6.683304552674629306, 4.336808689942017736E-16, -104.1296019027812321 ) ) ;
#1155 = CARTESIAN_POINT ( 'NONE',  ( -3.249999999999999112, 8.687499999999998224, -2.153805922287440833 ) ) ;
#1156 = ORIENTED_EDGE ( 'NONE', *, *, #11118, .T. ) ;
#1157 = CARTESIAN_POINT ( 'NONE',  ( -5.229219651426930682, 15.00000000000000000, -111.7283649856961318 ) ) ;
#1158 = PLANE ( 'NONE',  #8481 ) ;
#1159 = CARTESIAN_POINT ( 'NONE',  ( 9.068716941525991615, 0.000000000000000000, -163.1923081219560174 ) ) ;
#1160 = CARTESIAN_POINT ( 'NONE',  ( -3.249999999999999556, 0.2500000000000000000, -3.499999999999999556 ) ) ;
#1161 = CARTESIAN_POINT ( 'NONE',  ( 3.249999999999999556, 14.25000000000000178, -3.500000000000000000 ) ) ;
#1162 = CARTESIAN_POINT ( 'NONE',  ( 30.32986759126112730, 0.7500000000000000000, 41.04214087805579680 ) ) ;
#1163 = CARTESIAN_POINT ( 'NONE',  ( 1.553300858899105963, 3.062500000000000000, -7.250000000000000888 ) ) ;
#1164 = CARTESIAN_POINT ( 'NONE',  ( 0.2625675448779583032, 9.999999999999998224, 2.974107436473179877 ) ) ;
#1165 = DIRECTION ( 'NONE',  ( 0.000000000000000000, 0.000000000000000000, -1.000000000000000000 ) ) ;
#1166 = EDGE_CURVE ( 'NONE', #4807, #3224, #3390, .T. ) ;
#1167 = CARTESIAN_POINT ( 'NONE',  ( -12.27209645382210823, 9.999999999999998224, -127.2227734861304782 ) ) ;
#1168 = EDGE_CURVE ( 'NONE', #11237, #4454, #4051, .T. ) ;
#1169 = DIRECTION ( 'NONE',  ( 0.000000000000000000, 1.000000000000000000, 0.000000000000000000 ) ) ;
#1170 = CARTESIAN_POINT ( 'NONE',  ( -1.346194077712559389, 13.06250000000000000, -0.2500000000000002220 ) ) ;
#1171 = CARTESIAN_POINT ( 'NONE',  ( 4.856804767890293029, 14.90536770052035109, -1.840041787218291036 ) ) ;
#1172 = CARTESIAN_POINT ( 'NONE',  ( 5.079523875935373134, 5.000000000000000888, -108.2552591983082806 ) ) ;
#1173 = ORIENTED_EDGE ( 'NONE', *, *, #9323, .F. ) ;
#1174 = ORIENTED_EDGE ( 'NONE', *, *, #1793, .T. ) ;
#1175 = CARTESIAN_POINT ( 'NONE',  ( -5.131649475197874288, -6.588576144931190669E-14, -112.7947322869705289 ) ) ;
#1176 = CARTESIAN_POINT ( 'NONE',  ( 8.424062888332693788, 12.50000000000000178, -112.3245025925639169 ) ) ;
#1177 = CARTESIAN_POINT ( 'NONE',  ( -1.553300858899107295, 4.437500000000000888, -7.250000000000000000 ) ) ;
#1178 = CARTESIAN_POINT ( 'NONE',  ( -3.750000000000000000, 3.687500000000000444, -1.946699141100893149 ) ) ;
#1179 = CARTESIAN_POINT ( 'NONE',  ( -7.534724830571902565, 2.770061804015413626E-12, -106.8248685501869062 ) ) ;
#1180 = ORIENTED_EDGE ( 'NONE', *, *, #7997, .T. ) ;
#1181 = CARTESIAN_POINT ( 'NONE',  ( 3.249999999999999556, 2.249999999999999556, -3.500000000000000000 ) ) ;
#1182 = CARTESIAN_POINT ( 'NONE',  ( -1.653263949012559797, 5.000000000000000888, -106.3284344075506311 ) ) ;
#1183 = FACE_OUTER_BOUND ( 'NONE', #6773, .T. ) ;
#1184 = SHAPE_REPRESENTATION_RELATIONSHIP ( 'NONE' , 'NONE' ,  #9314, #2810 ) ;
#1185 = CARTESIAN_POINT ( 'NONE',  ( -3.249999999999999556, 5.312500000000001776, -4.846194077712557835 ) ) ;
#1186 = CARTESIAN_POINT ( 'NONE',  ( 10.32040002734018991, 12.49999999999999822, -106.4311084481271479 ) ) ;
#1187 = CARTESIAN_POINT ( 'NONE',  ( 4.114500516011223574, 1.734723475976807094E-15, -119.1606835011388767 ) ) ;
#1188 = ORIENTED_EDGE ( 'NONE', *, *, #9195, .T. ) ;
#1189 = EDGE_CURVE ( 'NONE', #5809, #1079, #10489, .T. ) ;
#1190 = CARTESIAN_POINT ( 'NONE',  ( -0.4126978180549508712, 14.99999999999999822, -116.4224499489989881 ) ) ;
#1191 = CARTESIAN_POINT ( 'NONE',  ( 1.346194077712558279, 13.56250000000000000, -6.750000000000000000 ) ) ;
#1192 = VERTEX_POINT ( 'NONE', #6942 ) ;
#1193 = EDGE_LOOP ( 'NONE', ( #9420, #5533, #9942, #4731, #12082, #12795, #2752, #1848 ) ) ;
#1194 = CARTESIAN_POINT ( 'NONE',  ( 7.113306724408225534, 2.331468351713773494E-16, 51.45871142768356066 ) ) ;
#1195 = CARTESIAN_POINT ( 'NONE',  ( 3.750000000000000000, 4.312500000000000000, -1.946699141100892705 ) ) ;
#1196 = CARTESIAN_POINT ( 'NONE',  ( -3.980102097228897738E-16, 7.000000000000000000, -6.749999999999999112 ) ) ;
#1197 = ORIENTED_EDGE ( 'NONE', *, *, #3286, .F. ) ;
#1198 = CARTESIAN_POINT ( 'NONE',  ( 6.172117187913792158, 13.05783589229790564, 4.248210876070234399 ) ) ;
#1199 = CARTESIAN_POINT ( 'NONE',  ( 3.249999999999998668, 2.687500000000000888, -4.846194077712560500 ) ) ;
#1200 = CARTESIAN_POINT ( 'NONE',  ( -12.27209645382210823, 2.500000000000000444, -127.2227734861304782 ) ) ;
#1201 = FACE_OUTER_BOUND ( 'NONE', #14682, .T. ) ;
#1202 = CARTESIAN_POINT ( 'NONE',  ( -6.119281984250456219, -2.490287375297125294, -44.38286699775952826 ) ) ;
#1203 = PERSON_AND_ORGANIZATION ( #3176, #3020 ) ;
#1204 = CARTESIAN_POINT ( 'NONE',  ( 31.03240854397274617, 8.773889247172311556, -47.17439748069210026 ) ) ;
#1205 = EDGE_CURVE ( 'NONE', #12491, #8603, #12753, .T. ) ;
#1206 = ORIENTED_EDGE ( 'NONE', *, *, #7217, .T. ) ;
#1207 = CARTESIAN_POINT ( 'NONE',  ( -10.29275726619094300, 0.000000000000000000, -34.56909192082969895 ) ) ;
#1208 = CARTESIAN_POINT ( 'NONE',  ( -1.553300858899106629, 11.56250000000000178, 0.2499999999999998335 ) ) ;
#1209 = CARTESIAN_POINT ( 'NONE',  ( -65.95160144704729532, 15.05880728265431578, -200.7665161391323352 ) ) ;
#1210 = CARTESIAN_POINT ( 'NONE',  ( -4.924771681124648026, 0.000000000000000000, -137.0932397189673111 ) ) ;
#1211 = CARTESIAN_POINT ( 'NONE',  ( -3.249999999999999112, 2.687500000000000888, -2.153805922287440833 ) ) ;
#1212 = CARTESIAN_POINT ( 'NONE',  ( 9.548749501005779905, 1.188659780561164281, -105.8881707746913037 ) ) ;
#1213 = APPROVAL_ROLE ( '' ) ;
#1214 = CC_DESIGN_SECURITY_CLASSIFICATION ( #13819, ( #5003 ) ) ;
#1215 = FACE_OUTER_BOUND ( 'NONE', #8276, .T. ) ;
#1216 = DIRECTION ( 'NONE',  ( 0.000000000000000000, -1.000000000000000000, 0.000000000000000000 ) ) ;
#1217 = VECTOR ( 'NONE', #7703, 1000.000000000000000 ) ;
#1218 = ORIENTED_EDGE ( 'NONE', *, *, #14526, .T. ) ;
#1219 = CARTESIAN_POINT ( 'NONE',  ( 6.010779701672017694, 3.744510043399113641, 5.110648605019955326 ) ) ;
#1220 = CARTESIAN_POINT ( 'NONE',  ( 1.346194077712558279, 1.562500000000000000, -6.750000000000000000 ) ) ;
#1221 =( BOUNDED_SURFACE ( )  B_SPLINE_SURFACE ( 3, 2, ( 
 ( #5378, #4446, #3060 ),
 ( #12719, #13804, #13887 ),
 ( #7772, #12562, #13733 ),
 ( #14827, #744, #9007 ),
 ( #3204, #5452, #10092 ),
 ( #7921, #12485, #10313 ),
 ( #4226, #14979, #1975 ),
 ( #9159, #7998, #6690 ),
 ( #12641, #9083, #3132 ),
 ( #4526, #7846, #3358 ),
 ( #6767, #5528, #10247 ),
 ( #2130, #11480, #9235 ),
 ( #14906, #898, #5599 ),
 ( #15052, #6833, #3283 ),
 ( #11549, #8932, #8069 ),
 ( #965, #5672, #1615 ),
 ( #6327, #11251, #672 ),
 ( #13660, #1903, #4303 ) ),
 .UNSPECIFIED., .F., .F., .T. ) 
 B_SPLINE_SURFACE_WITH_KNOTS ( ( 4, 2, 2, 2, 2, 2, 2, 2, 4 ),
 ( 3, 3 ),
 ( -1.268724681189376368E-05, 0.001841763813947226193, 0.002768989344326786180, 0.003696214874706346167, 0.004623440405085906153, 0.005087053170275686147, 0.005550665935465466140, 0.006477891465845026127, 0.007405116996224586114 ),
 ( 0.000000000000000000, 1.000000000000000000 ),
 .UNSPECIFIED. ) 
 GEOMETRIC_REPRESENTATION_ITEM ( )  RATIONAL_B_SPLINE_SURFACE ( (
 ( 1.000000000000000000, 1.000000000000000000, 1.000000000000000000),
 ( 1.000000000000000000, 0.9999613041041146566, 1.000000000000000000),
 ( 1.000000000000000000, 0.9910800145946376816, 1.000000000000000000),
 ( 1.000000000000000000, 0.9642327837277934188, 1.000000000000000000),
 ( 1.000000000000000000, 0.9530488795586037343, 1.000000000000000000),
 ( 1.000000000000000000, 0.9269314470905131165, 1.000000000000000000),
 ( 1.000000000000000000, 0.9119402567601512244, 1.000000000000000000),
 ( 1.000000000000000000, 0.8786186012477549268, 1.000000000000000000),
 ( 1.000000000000000000, 0.8602835836478229803, 1.000000000000000000),
 ( 1.000000000000000000, 0.8324170639630756874, 1.000000000000000000),
 ( 1.000000000000000000, 0.8230360448555069652, 1.000000000000000000),
 ( 1.000000000000000000, 0.8044254825442935797, 1.000000000000000000),
 ( 1.000000000000000000, 0.7951379861664216175, 1.000000000000000000),
 ( 1.000000000000000000, 0.7688101143225162248, 1.000000000000000000),
 ( 1.000000000000000000, 0.7531508686541504849, 1.000000000000000000),
 ( 1.000000000000000000, 0.7304464755382781282, 1.000000000000000000),
 ( 1.000000000000000000, 0.7240603277304887841, 1.000000000000000000),
 ( 1.000000000000000000, 0.7240860691865900201, 1.000000000000000000) ) ) 
 REPRESENTATION_ITEM ( '' )  SURFACE ( )  );
#1222 = CARTESIAN_POINT ( 'NONE',  ( -65.40294475132493801, 15.00000000000000000, -186.2934539482498337 ) ) ;
#1223 = CARTESIAN_POINT ( 'NONE',  ( -2.298097038856278029, 5.625000000000000888, -1.201902961143720638 ) ) ;
#1224 = ORIENTED_EDGE ( 'NONE', *, *, #8081, .T. ) ;
#1225 = CARTESIAN_POINT ( 'NONE',  ( -5.447453277355505108, 9.999999999999998224, -116.0587048211077814 ) ) ;
#1226 = UNCERTAINTY_MEASURE_WITH_UNIT (LENGTH_MEASURE( 1.000000000000000082E-05 ), #10465, 'distance_accuracy_value', 'NONE');
#1227 = CARTESIAN_POINT ( 'NONE',  ( 38.58381714758451864, 1.749999999999999778, 41.14817863027235489 ) ) ;
#1228 = CC_DESIGN_APPROVAL ( #9706, ( #12585 ) ) ;
#1229 = CARTESIAN_POINT ( 'NONE',  ( 9.112379365197755376, 14.99999999812265727, -105.9782736279704238 ) ) ;
#1230 = CARTESIAN_POINT ( 'NONE',  ( -1.346194077712559389, 1.437500000000000000, -6.749999999999999112 ) ) ;
#1231 = CIRCLE ( 'NONE', #7168, 1.000000000000000222 ) ;
#1232 = CARTESIAN_POINT ( 'NONE',  ( -1.553300858899106629, 1.562500000000000222, 0.2499999999999998335 ) ) ;
#1233 = AXIS2_PLACEMENT_3D ( 'NONE', #6432, #2733, #7667 ) ;
#1234 = CARTESIAN_POINT ( 'NONE',  ( 2.651650429449553759, 4.875000000000000000, -0.8483495705504471296 ) ) ;
#1235 = CARTESIAN_POINT ( 'NONE',  ( 1.171458888995337677, 8.673617379884035472E-16, -111.2928373221764531 ) ) ;
#1236 = CARTESIAN_POINT ( 'NONE',  ( 1.553300858899105963, 4.062500000000001776, -7.250000000000000888 ) ) ;
#1237 = DIRECTION ( 'NONE',  ( -0.000000000000000000, 0.000000000000000000, 1.000000000000000000 ) ) ;
#1238 = DIRECTION ( 'NONE',  ( 0.000000000000000000, 0.000000000000000000, -1.000000000000000000 ) ) ;
#1239 = PLANE ( 'NONE',  #12508 ) ;
#1240 = EDGE_CURVE ( 'NONE', #6640, #10252, #1332, .T. ) ;
#1241 = CARTESIAN_POINT ( 'NONE',  ( 4.261909775985413873, 13.80603281949575845, 3.020287175281327841 ) ) ;
#1242 = CARTESIAN_POINT ( 'NONE',  ( -1.346194077712559389, 11.06250000000000000, -0.2500000000000002220 ) ) ;
#1243 = AXIS2_PLACEMENT_3D ( 'NONE', #11059, #1786, #6270 ) ;
#1244 = CIRCLE ( 'NONE', #12616, 0.2500000000000002220 ) ;
#1245 = CARTESIAN_POINT ( 'NONE',  ( -8.512178793150408040, 12.56551871291872580, -104.4358902311836914 ) ) ;
#1246 = CARTESIAN_POINT ( 'NONE',  ( 4.586790536111674754, 8.673617379884035472E-16, -116.5616331785999762 ) ) ;
#1247 = VECTOR ( 'NONE', #11189, 1000.000000000000000 ) ;
#1248 = ORIENTED_EDGE ( 'NONE', *, *, #8460, .F. ) ;
#1249 = ORIENTED_EDGE ( 'NONE', *, *, #5177, .T. ) ;
#1250 = CARTESIAN_POINT ( 'NONE',  ( -2.641315011715085426, 4.336808689942017736E-16, -114.1979735927311879 ) ) ;
#1251 = LINE ( 'NONE', #12932, #7716 ) ;
#1252 = CARTESIAN_POINT ( 'NONE',  ( 1.553300858899105963, 3.562500000000000444, -7.250000000000000888 ) ) ;
#1253 = CARTESIAN_POINT ( 'NONE',  ( -1.553300858899107073, 5.937500000000000000, -7.249999999999999112 ) ) ;
#1254 = CARTESIAN_POINT ( 'NONE',  ( -0.3766621274091715987, 0.5000000000000000000, -6.863050255469941519 ) ) ;
#1255 = VERTEX_POINT ( 'NONE', #8176 ) ;
#1256 = EDGE_CURVE ( 'NONE', #6645, #6005, #2991, .T. ) ;
#1257 = ADVANCED_FACE ( 'NONE', ( #9040 ), #3159, .F. ) ;
#1258 = CARTESIAN_POINT ( 'NONE',  ( 2.298097038856279362, 1.375000000000000000, -1.201902961143720860 ) ) ;
#1259 = VECTOR ( 'NONE', #7800, 1000.000000000000000 ) ;
#1260 = AXIS2_PLACEMENT_3D ( 'NONE', #2358, #4748, #6133 ) ;
#1261 = CARTESIAN_POINT ( 'NONE',  ( -47.98141941977416280, 15.00000000000000000, -149.0590141369269759 ) ) ;
#1262 = DIRECTION ( 'NONE',  ( -0.000000000000000000, -1.000000000000000000, -0.000000000000000000 ) ) ;
#1263 = CARTESIAN_POINT ( 'NONE',  ( -3.249999999999999556, 4.250000000000000000, -3.499999999999999556 ) ) ;
#1264 = CARTESIAN_POINT ( 'NONE',  ( -9.739626904459422363, 10.00000000000000000, -116.2879091882953446 ) ) ;
#1265 = CARTESIAN_POINT ( 'NONE',  ( 1.243260443319662123, 4.000000000000000000, -139.4020581015306846 ) ) ;
#1266 = CARTESIAN_POINT ( 'NONE',  ( 30.32986759126112730, 0.000000000000000000, 45.04214087805580391 ) ) ;
#1267 = ORIENTED_EDGE ( 'NONE', *, *, #557, .F. ) ;
#1268 = CARTESIAN_POINT ( 'NONE',  ( -3.194662295375430894, 15.00000000000000178, -123.6199554999345764 ) ) ;
#1269 = CARTESIAN_POINT ( 'NONE',  ( -3.249999999999999556, 13.25000000000000000, -3.499999999999999556 ) ) ;
#1270 = VECTOR ( 'NONE', #8112, 1000.000000000000000 ) ;
#1271 = ORIENTED_EDGE ( 'NONE', *, *, #2692, .F. ) ;
#1272 = ORIENTED_EDGE ( 'NONE', *, *, #2054, .T. ) ;
#1273 = CARTESIAN_POINT ( 'NONE',  ( 0.000000000000000000, 5.000000000000000000, 0.000000000000000000 ) ) ;
#1274 = CARTESIAN_POINT ( 'NONE',  ( -1.553300858899107073, 3.937500000000001332, -7.249999999999999112 ) ) ;
#1275 = CARTESIAN_POINT ( 'NONE',  ( 0.000000000000000000, 12.50000000000000178, -0.2500000000000002220 ) ) ;
#1276 = EDGE_LOOP ( 'NONE', ( #12705, #2489, #6368, #3902, #4448 ) ) ;
#1277 = CARTESIAN_POINT ( 'NONE',  ( -1.030030362071697070, 15.00000000000000000, -105.0143096063705315 ) ) ;
#1278 = CARTESIAN_POINT ( 'NONE',  ( 3.249999999999999112, 4.812500000000000888, -2.153805922287439945 ) ) ;
#1279 = PRODUCT_DEFINITION_SHAPE ( 'NONE', 'NONE',  #15323 ) ;
#1280 = EDGE_CURVE ( 'NONE', #12491, #602, #5926, .T. ) ;
#1281 = AXIS2_PLACEMENT_3D ( 'NONE', #1438, #6144, #1517 ) ;
#1282 = CARTESIAN_POINT ( 'NONE',  ( -8.698259420408664511, 0.9528231151539969801, -104.5458497525427077 ) ) ;
#1283 = CARTESIAN_POINT ( 'NONE',  ( 11.86236191862562706, 1.294159459973254878, -165.2395099304358723 ) ) ;
#1284 = CARTESIAN_POINT ( 'NONE',  ( 6.803763450426751014, 15.00000000000000000, -119.3127978128359530 ) ) ;
#1285 = APPLICATION_PROTOCOL_DEFINITION ( 'international standard', 'config_control_design', 1994, #5805 ) ;
#1286 = DIRECTION ( 'NONE',  ( 0.9997619372588932851, -0.000000000000000000, 0.02181900108494707474 ) ) ;
#1287 = ORIENTED_EDGE ( 'NONE', *, *, #6290, .F. ) ;
#1288 = AXIS2_PLACEMENT_3D ( 'NONE', #1342, #572, #11152 ) ;
#1289 = DIRECTION ( 'NONE',  ( -0.9997619372588931741, -0.000000000000000000, -0.02181900108494707127 ) ) ;
#1290 = EDGE_CURVE ( 'NONE', #13945, #6914, #8284, .T. ) ;
#1291 = CARTESIAN_POINT ( 'NONE',  ( 3.749999999999999556, 14.25000000000000178, -3.500000000000000444 ) ) ;
#1292 = EDGE_CURVE ( 'NONE', #814, #12909, #2740, .T. ) ;
#1293 = CARTESIAN_POINT ( 'NONE',  ( 1.086818044140344774, 4.588323854676484181, -139.4449740270702591 ) ) ;
#1294 = EDGE_CURVE ( 'NONE', #4481, #15113, #12104, .T. ) ;
#1295 = CARTESIAN_POINT ( 'NONE',  ( -64.28343470285902583, 14.09174185945640190, -209.5512319406730342 ) ) ;
#1296 = CARTESIAN_POINT ( 'NONE',  ( 0.000000000000000000, 5.000000000000000888, -100.6237003951525537 ) ) ;
#1297 = CARTESIAN_POINT ( 'NONE',  ( 3.249999999999998224, 2.312500000000000000, -2.153805922287439945 ) ) ;
#1298 = CARTESIAN_POINT ( 'NONE',  ( 6.918686878921664452, 0.02960220130170718167, -105.2168480447504493 ) ) ;
#1299 = DATE_AND_TIME ( #4850, #14377 ) ;
#1300 = CARTESIAN_POINT ( 'NONE',  ( -5.309262520577839872, 13.36526483154179523, -125.0911079416483176 ) ) ;
#1301 = LINE ( 'NONE', #14461, #11856 ) ;
#1302 = ORIENTED_EDGE ( 'NONE', *, *, #11838, .T. ) ;
#1303 = CARTESIAN_POINT ( 'NONE',  ( 4.165066839799179021, 0.2629148108822390584, 0.5887562915265751595 ) ) ;
#1304 = CARTESIAN_POINT ( 'NONE',  ( 3.249999999999998668, 3.687500000000000444, -4.846194077712560500 ) ) ;
#1305 = VECTOR ( 'NONE', #13119, 1000.000000000000000 ) ;
#1306 = CARTESIAN_POINT ( 'NONE',  ( -8.643796269099508933, 1.337050190792271387, -105.3552258418637706 ) ) ;
#1307 = CARTESIAN_POINT ( 'NONE',  ( 3.249999999999999556, 7.250000000000001776, -3.500000000000000000 ) ) ;
#1308 = VERTEX_POINT ( 'NONE', #7081 ) ;
#1309 = CARTESIAN_POINT ( 'NONE',  ( -6.422940335516989840, 9.999999999999998224, -108.3014594335602112 ) ) ;
#1310 = CARTESIAN_POINT ( 'NONE',  ( 3.787708185468225519, 14.86616054401451414, -0.8541222820799866389 ) ) ;
#1311 = CARTESIAN_POINT ( 'NONE',  ( -10.50399746308849913, 15.00000000000000000, -142.5005062768871653 ) ) ;
#1312 = CARTESIAN_POINT ( 'NONE',  ( -3.980102097228897245E-16, 0.5000000000000000000, -6.749999999999999112 ) ) ;
#1313 = CARTESIAN_POINT ( 'NONE',  ( -3.749999999999999556, 2.750000000000000444, -3.499999999999999112 ) ) ;
#1314 = CARTESIAN_POINT ( 'NONE',  ( 3.749999999999999112, 5.687500000000000000, -5.053300858899108405 ) ) ;
#1315 = CC_DESIGN_PERSON_AND_ORGANIZATION_ASSIGNMENT ( #52, #15294, ( #10487 ) ) ;
#1316 = CARTESIAN_POINT ( 'NONE',  ( -4.234402844927150689, 0.000000000000000000, -117.4888040839639558 ) ) ;
#1317 = CARTESIAN_POINT ( 'NONE',  ( -2.651650429449552870, 5.625000000000000888, -0.8483495705504463524 ) ) ;
#1318 = AXIS2_PLACEMENT_3D ( 'NONE', #5046, #176, #101 ) ;
#1319 = CARTESIAN_POINT ( 'NONE',  ( 2.198198389973041955, 14.05584352655475122, 1.458542947118257604 ) ) ;
#1320 = VECTOR ( 'NONE', #10549, 1000.000000000000000 ) ;
#1321 = CARTESIAN_POINT ( 'NONE',  ( -3.836704105290339228, 11.25565849803658125, -45.28046668454305035 ) ) ;
#1322 =( BOUNDED_SURFACE ( )  B_SPLINE_SURFACE ( 3, 2, ( 
 ( #7539, #12256, #8782 ),
 ( #1744, #11320, #9154 ),
 ( #14753, #8850, #13729 ),
 ( #3056, #5522, #12558 ),
 ( #7610, #7768, #10243 ),
 ( #4151, #11474, #3198 ),
 ( #5447, #1824, #12635 ),
 ( #9078, #5305, #4440 ),
 ( #3129, #14975, #13656 ),
 ( #8927, #15046, #10089 ),
 ( #13578, #11248, #12482 ),
 ( #7842, #4222, #1971 ),
 ( #740, #2907, #7690 ),
 ( #6686, #893, #1899 ),
 ( #12325, #6613, #10167 ),
 ( #14901, #13799, #4297 ) ),
 .UNSPECIFIED., .F., .F., .T. ) 
 B_SPLINE_SURFACE_WITH_KNOTS ( ( 4, 2, 2, 2, 2, 2, 2, 4 ),
 ( 3, 3 ),
 ( -1.334638064060296792E-05, 0.001685485362004357284, 0.002534901233326837446, 0.003384317104649317391, 0.004233732975971796902, 0.005083148847294277281, 0.005932564718616757660, 0.006781980589939238038 ),
 ( 0.000000000000000000, 1.000000000000000000 ),
 .UNSPECIFIED. ) 
 GEOMETRIC_REPRESENTATION_ITEM ( )  RATIONAL_B_SPLINE_SURFACE ( (
 ( 1.000000000000000000, 1.000000000000000000, 1.000000000000000000),
 ( 1.000000000000000000, 0.9999849372740239328, 1.000000000000000000),
 ( 1.000000000000000000, 0.9937682810188976923, 1.000000000000000000),
 ( 1.000000000000000000, 0.9761755817002490954, 1.000000000000000000),
 ( 1.000000000000000000, 0.9688601978537569881, 1.000000000000000000),
 ( 1.000000000000000000, 0.9524575494629958783, 1.000000000000000000),
 ( 1.000000000000000000, 0.9433181971012551958, 1.000000000000000000),
 ( 1.000000000000000000, 0.9239129119548288305, 1.000000000000000000),
 ( 1.000000000000000000, 0.9135210720624407088, 1.000000000000000000),
 ( 1.000000000000000000, 0.8936014670381493552, 1.000000000000000000),
 ( 1.000000000000000000, 0.8840084896217472732, 1.000000000000000000),
 ( 1.000000000000000000, 0.8670987394474829468, 1.000000000000000000),
 ( 1.000000000000000000, 0.8600561105956968655, 1.000000000000000000),
 ( 1.000000000000000000, 0.8503557397562589992, 1.000000000000000000),
 ( 1.000000000000000000, 0.8476417977143253513, 1.000000000000000000),
 ( 1.000000000000000000, 0.8476602389432602580, 1.000000000000000000) ) ) 
 REPRESENTATION_ITEM ( '' )  SURFACE ( )  );
#1323 = CARTESIAN_POINT ( 'NONE',  ( -8.886921396801742645, 2.500000000000000444, -105.5168766094550676 ) ) ;
#1324 = DIRECTION ( 'NONE',  ( -0.02181900108494732801, 0.000000000000000000, 0.9997619372588931741 ) ) ;
#1325 = CARTESIAN_POINT ( 'NONE',  ( 2.298097038856278473, 10.62500000000000000, -5.798097038856279362 ) ) ;
#1326 = CARTESIAN_POINT ( 'NONE',  ( -7.434246213560691707, 13.81406867328371746, -104.1118743468900050 ) ) ;
#1327 = FACE_OUTER_BOUND ( 'NONE', #9612, .T. ) ;
#1328 = EDGE_LOOP ( 'NONE', ( #1206, #5247, #11489 ) ) ;
#1329 = CARTESIAN_POINT ( 'NONE',  ( -2.651650429449553314, 7.874999999999999112, -6.151650429449552426 ) ) ;
#1330 = ORIENTED_EDGE ( 'NONE', *, *, #749, .F. ) ;
#1331 = CARTESIAN_POINT ( 'NONE',  ( -6.399074641068315472, 7.806255641895631925E-15, -108.4234853096273099 ) ) ;
#1332 = CIRCLE ( 'NONE', #7085, 0.5000000000000004441 ) ;
#1333 = CARTESIAN_POINT ( 'NONE',  ( 8.475206276408092876, -1.020558061026470176, -34.56909192082981974 ) ) ;
#1334 = CARTESIAN_POINT ( 'NONE',  ( 2.651650429449553759, 6.875000000000000000, -0.8483495705504471296 ) ) ;
#1335 = CARTESIAN_POINT ( 'NONE',  ( 0.000000000000000000, 4.499999999999999112, 0.2499999999999998057 ) ) ;
#1336 = VECTOR ( 'NONE', #1872, 1000.000000000000000 ) ;
#1337 = CARTESIAN_POINT ( 'NONE',  ( 1.635615696801046015, 1.750000000000000000, -0.6802899045268993028 ) ) ;
#1338 = ORIENTED_EDGE ( 'NONE', *, *, #11568, .F. ) ;
#1339 = CARTESIAN_POINT ( 'NONE',  ( -2.298097038856279362, 2.875000000000000000, -5.798097038856278473 ) ) ;
#1340 = CARTESIAN_POINT ( 'NONE',  ( -59.94788933440509737, 15.00000000000000000, -157.3141654283494120 ) ) ;
#1341 = DIRECTION ( 'NONE',  ( 1.000000000000000000, 0.000000000000000000, 0.000000000000000000 ) ) ;
#1342 = CARTESIAN_POINT ( 'NONE',  ( 0.000000000000000000, 0.000000000000000000, 0.000000000000000000 ) ) ;
#1343 = CARTESIAN_POINT ( 'NONE',  ( -1.346194077712559389, 9.062499999999998224, -0.2500000000000002220 ) ) ;
#1344 = VECTOR ( 'NONE', #9791, 1000.000000000000227 ) ;
#1345 = CARTESIAN_POINT ( 'NONE',  ( -6.338840459740750610, 9.999999999966100006, -126.0591383734726350 ) ) ;
#1346 = CARTESIAN_POINT ( 'NONE',  ( -2.035316908179384932, 4.336808689942018525E-15, -133.6663417170241246 ) ) ;
#1347 = CARTESIAN_POINT ( 'NONE',  ( 24.24946450389425934, 8.673617379884035472E-16, -141.2402007109023145 ) ) ;
#1348 = ORIENTED_EDGE ( 'NONE', *, *, #12802, .T. ) ;
#1349 = LINE ( 'NONE', #4826, #1358 ) ;
#1350 = DIRECTION ( 'NONE',  ( -0.000000000000000000, 1.000000000000000000, -0.000000000000000000 ) ) ;
#1351 = ORIENTED_EDGE ( 'NONE', *, *, #8138, .T. ) ;
#1352 = VERTEX_POINT ( 'NONE', #4706 ) ;
#1353 = CYLINDRICAL_SURFACE ( 'NONE', #4541, 3.500000000000000000 ) ;
#1354 = CARTESIAN_POINT ( 'NONE',  ( -2.651650429449553314, 6.875000000000000000, -6.151650429449552426 ) ) ;
#1355 = CARTESIAN_POINT ( 'NONE',  ( 3.249999999999999556, 9.249999999999998224, -3.500000000000000000 ) ) ;
#1356 = VERTEX_POINT ( 'NONE', #9418 ) ;
#1357 = CARTESIAN_POINT ( 'NONE',  ( 6.122889832264990062, 9.999999999999998224, 5.281130614573720905 ) ) ;
#1358 = VECTOR ( 'NONE', #3512, 1000.000000000000227 ) ;
#1359 = CARTESIAN_POINT ( 'NONE',  ( 2.298097038856279362, 5.875000000000000000, -1.201902961143720860 ) ) ;
#1360 = CARTESIAN_POINT ( 'NONE',  ( -24.91286313170930100, 3.952717365971852637, -209.6104391265338904 ) ) ;
#1361 = CARTESIAN_POINT ( 'NONE',  ( -40.67260926563410806, 10.00000000000000178, -157.6318504523734703 ) ) ;
#1362 = CARTESIAN_POINT ( 'NONE',  ( -67.58382170693636226, 10.00000000000000000, -204.5178482451963191 ) ) ;
#1363 = CALENDAR_DATE ( 2026, 8, 10 ) ;
#1364 = DIRECTION ( 'NONE',  ( 0.000000000000000000, 0.000000000000000000, 1.000000000000000000 ) ) ;
#1365 = ORIENTED_EDGE ( 'NONE', *, *, #14365, .T. ) ;
#1366 = ADVANCED_FACE ( 'NONE', ( #9731 ), #1453, .F. ) ;
#1367 = CARTESIAN_POINT ( 'NONE',  ( 1.346194077712558057, 9.562500000000000000, -6.750000000000000000 ) ) ;
#1368 =( REPRESENTATION_RELATIONSHIP ('NONE','NONE', #11394, #10790 ) REPRESENTATION_RELATIONSHIP_WITH_TRANSFORMATION ( #3424 )SHAPE_REPRESENTATION_RELATIONSHIP( ) );
#1369 = CARTESIAN_POINT ( 'NONE',  ( 17.56616871422910009, 8.749999999999998224, -94.70022032590149763 ) ) ;
#1370 = CARTESIAN_POINT ( 'NONE',  ( 1.553300858899105963, 13.06250000000000178, -7.249999999999999112 ) ) ;
#1371 = CC_DESIGN_PERSON_AND_ORGANIZATION_ASSIGNMENT ( #8795, #14768, ( #9187 ) ) ;
#1372 = CARTESIAN_POINT ( 'NONE',  ( 1.004149434879655356, 4.793811891163896277, -139.4756852570866954 ) ) ;
#1373 = CARTESIAN_POINT ( 'NONE',  ( -63.21422129964969372, 10.11977001910463869, -203.6040552221171254 ) ) ;
#1374 = DIRECTION ( 'NONE',  ( -0.000000000000000000, 1.000000000000000000, -0.000000000000000000 ) ) ;
#1375 = CARTESIAN_POINT ( 'NONE',  ( 1.346194077712558279, 2.062500000000000000, -6.750000000000000888 ) ) ;
#1376 = CARTESIAN_POINT ( 'NONE',  ( 9.135126988672782389, 15.00000000000142819, -105.9368265145316457 ) ) ;
#1377 = APPROVAL_DATE_TIME ( #8396, #6183 ) ;
#1378 = B_SPLINE_CURVE_WITH_KNOTS ( 'NONE', 3,
 ( #1954, #13943, #12543, #14014, #15034, #6747 ),
 .UNSPECIFIED., .F., .F.,
 ( 4, 2, 4 ),
 ( 1.551583845779545699E-17, 0.006357786140926138634, 0.01271557228185226165 ),
 .UNSPECIFIED. ) ;
#1379 = CARTESIAN_POINT ( 'NONE',  ( -3.490754879379053044, 14.52642831644817711, -125.2917343356935476 ) ) ;
#1380 = DIRECTION ( 'NONE',  ( -0.000000000000000000, -1.000000000000000000, -0.000000000000000000 ) ) ;
#1381 = ORIENTED_EDGE ( 'NONE', *, *, #14526, .F. ) ;
#1382 = CARTESIAN_POINT ( 'NONE',  ( 5.779749278148204716, 0.3260126679219001455, 0.3456447915639645485 ) ) ;
#1383 = CARTESIAN_POINT ( 'NONE',  ( -3.249999999999999556, 7.187500000000000000, -2.153805922287440833 ) ) ;
#1384 = EDGE_CURVE ( 'NONE', #13806, #12909, #13290, .T. ) ;
#1385 = CARTESIAN_POINT ( 'NONE',  ( -9.094070923552267871, 1.650112951200696232, -104.6311941295649177 ) ) ;
#1386 = CARTESIAN_POINT ( 'NONE',  ( -3.249999999999999556, 0.7499999999999998890, -3.500000000000000000 ) ) ;
#1387 = CARTESIAN_POINT ( 'NONE',  ( -3.249999999999999112, 6.812500000000001776, -4.846194077712558723 ) ) ;
#1388 = CARTESIAN_POINT ( 'NONE',  ( -0.7574197398874851217, 14.99999999999999822, -108.9338761800286051 ) ) ;
#1389 = CARTESIAN_POINT ( 'NONE',  ( 1.638000757872857260, 13.54559192810887680, 1.952774218784175231 ) ) ;
#1390 = CARTESIAN_POINT ( 'NONE',  ( 1.818681402053747842, 9.999999999999998224, -137.3269588978967590 ) ) ;
#1391 = DIRECTION ( 'NONE',  ( 0.9997619372588931741, 0.000000000000000000, 0.02181900108494707474 ) ) ;
#1392 = CARTESIAN_POINT ( 'NONE',  ( 0.000000000000000000, 2.500000000000000000, 0.2499999999999998057 ) ) ;
#1393 = CARTESIAN_POINT ( 'NONE',  ( -2.651650429449552870, 6.125000000000000000, -0.8483495705504462414 ) ) ;
#1394 = CARTESIAN_POINT ( 'NONE',  ( -4.210400098449615491, 10.37725045066806295, -47.82562292290668893 ) ) ;
#1395 = CARTESIAN_POINT ( 'NONE',  ( -2.651650429449552870, 4.625000000000000888, -0.8483495705504463524 ) ) ;
#1396 = CARTESIAN_POINT ( 'NONE',  ( 0.8058036530323656743, 11.95234907359183296, 5.394660120521390212 ) ) ;
#1397 = CARTESIAN_POINT ( 'NONE',  ( 0.000000000000000000, 4.000000000000000000, 0.000000000000000000 ) ) ;
#1398 = CARTESIAN_POINT ( 'NONE',  ( -47.48189921986827500, 5.000000000000000000, -141.5723758807981483 ) ) ;
#1399 = CARTESIAN_POINT ( 'NONE',  ( 2.298097038856279362, 13.87500000000000000, -1.201902961143720860 ) ) ;
#1400 = EDGE_CURVE ( 'NONE', #5040, #11885, #1301, .T. ) ;
#1401 = CARTESIAN_POINT ( 'NONE',  ( 5.158994870041119007, 0.1324197759708019839, -0.7446863678409911813 ) ) ;
#1402 = CARTESIAN_POINT ( 'NONE',  ( -63.84637985160913587, 14.99926611874769478, -181.3101853188241535 ) ) ;
#1403 = CIRCLE ( 'NONE', #15249, 14.80000000000025651 ) ;
#1404 = VERTEX_POINT ( 'NONE', #3775 ) ;
#1405 = PRODUCT_DEFINITION_SHAPE ( 'NONE', 'NONE',  #15319 ) ;
#1406 = CARTESIAN_POINT ( 'NONE',  ( 3.749999999999999112, 10.18750000000000533, -5.053300858899108405 ) ) ;
#1407 = ORIENTED_EDGE ( 'NONE', *, *, #4989, .F. ) ;
#1408 = CARTESIAN_POINT ( 'NONE',  ( -4.554948446345685298, 4.336808689942017736E-16, -106.6475783469824847 ) ) ;
#1409 = CARTESIAN_POINT ( 'NONE',  ( -9.030574454602202650, -2.490287375297126626, -34.97919997656153157 ) ) ;
#1410 = CARTESIAN_POINT ( 'NONE',  ( 1.553300858899105963, 10.56250000000000000, -7.250000000000000888 ) ) ;
#1411 = CARTESIAN_POINT ( 'NONE',  ( -1.553300858899107073, 3.937500000000000444, -7.249999999999999112 ) ) ;
#1412 = CARTESIAN_POINT ( 'NONE',  ( -18.07331279040889882, 2.111503226455494708, -129.3631649207090675 ) ) ;
#1413 = VERTEX_POINT ( 'NONE', #5853 ) ;
#1414 = CARTESIAN_POINT ( 'NONE',  ( 1.346194077712558279, 5.062500000000000000, -6.750000000000000888 ) ) ;
#1415 = CARTESIAN_POINT ( 'NONE',  ( -3.750000000000000000, 8.250000000000000000, -3.499999999999999112 ) ) ;
#1416 = CLOSED_SHELL ( 'NONE', ( #7233, #7342, #7908, #10328, #15168, #10833, #14727, #3095, #12647, #10715 ) ) ;
#1417 = CARTESIAN_POINT ( 'NONE',  ( -69.36122292246929533, 15.00000000000000000, -183.5207230678662143 ) ) ;
#1418 = CARTESIAN_POINT ( 'NONE',  ( 3.528837229168438228, 8.673617379884037444E-16, -111.3086135701104098 ) ) ;
#1419 =( LENGTH_UNIT ( ) NAMED_UNIT ( * ) SI_UNIT ( .MILLI., .METRE. ) );
#1420 = CARTESIAN_POINT ( 'NONE',  ( -3.249999999999999556, 6.312500000000000888, -4.846194077712557835 ) ) ;
#1421 = CARTESIAN_POINT ( 'NONE',  ( -9.210337242380925105, 15.00000000000325961, -118.3325445941422629 ) ) ;
#1422 = COORDINATED_UNIVERSAL_TIME_OFFSET ( 0, 0, .AHEAD. ) ;
#1423 = CARTESIAN_POINT ( 'NONE',  ( -7.626890066890017472, 7.986110130110988110E-13, -122.9684017742491733 ) ) ;
#1424 = CARTESIAN_POINT ( 'NONE',  ( 8.173762862391447115, 8.673617379884035472E-16, -127.0422273781799731 ) ) ;
#1425 = VERTEX_POINT ( 'NONE', #8399 ) ;
#1426 = DIRECTION ( 'NONE',  ( 0.08794243244722413366, 0.000000000000000000, 0.9961255586397056438 ) ) ;
#1427 = CYLINDRICAL_SURFACE ( 'NONE', #1260, 2.500000000000000000 ) ;
#1428 = ORIENTED_EDGE ( 'NONE', *, *, #6458, .F. ) ;
#1429 = VERTEX_POINT ( 'NONE', #13048 ) ;
#1430 = CARTESIAN_POINT ( 'NONE',  ( 23.12860366745965734, 2.331468351712828833E-16, 67.62772795920155033 ) ) ;
#1431 = CARTESIAN_POINT ( 'NONE',  ( -4.592425496802573972E-16, 11.00000000000000178, -7.250000000000000000 ) ) ;
#1432 = CARTESIAN_POINT ( 'NONE',  ( 1.346194077712561166, 7.437499999999999112, -0.2500000000000011102 ) ) ;
#1433 = CARTESIAN_POINT ( 'NONE',  ( -2.298097038856278029, 11.62500000000000000, -1.201902961143720638 ) ) ;
#1434 = ORIENTED_EDGE ( 'NONE', *, *, #9620, .T. ) ;
#1435 = CARTESIAN_POINT ( 'NONE',  ( -22.96679436062313329, 8.673617379884035472E-16, -195.3937102046874941 ) ) ;
#1436 = CARTESIAN_POINT ( 'NONE',  ( -1.346194077712559389, 6.437500000000000888, -6.749999999999999112 ) ) ;
#1437 = CARTESIAN_POINT ( 'NONE',  ( 4.507463604512255806, 0.000000000000000000, 2.585105772303601945 ) ) ;
#1438 = CARTESIAN_POINT ( 'NONE',  ( -4.018470066652908734, 7.379999999999995453, -45.51728475810764962 ) ) ;
#1439 = DIRECTION ( 'NONE',  ( 0.000000000000000000, 0.000000000000000000, 1.000000000000000000 ) ) ;
#1440 = COORDINATED_UNIVERSAL_TIME_OFFSET ( 0, 0, .AHEAD. ) ;
#1441 = CARTESIAN_POINT ( 'NONE',  ( -24.70666345413006582, 3.149294185761901677, -208.4902367515576032 ) ) ;
#1442 = EDGE_LOOP ( 'NONE', ( #2948, #5754, #2966, #10415, #54, #3293 ) ) ;
#1443 = CARTESIAN_POINT ( 'NONE',  ( -3.249999999999999556, 2.250000000000000444, -3.499999999999999556 ) ) ;
#1444 = FACE_OUTER_BOUND ( 'NONE', #13418, .T. ) ;
#1445 = CARTESIAN_POINT ( 'NONE',  ( 3.749999999999999112, 15.31250000000000355, -1.946699141100893149 ) ) ;
#1446 = EDGE_CURVE ( 'NONE', #12487, #2721, #6437, .T. ) ;
#1447 = CARTESIAN_POINT ( 'NONE',  ( -67.58603348964146562, 10.40788280224345463, -204.4791092025774901 ) ) ;
#1448 = DIRECTION ( 'NONE',  ( -0.9997619372588931741, -0.000000000000000000, -0.02181900108494707127 ) ) ;
#1449 = CARTESIAN_POINT ( 'NONE',  ( 3.249999999999998224, 3.312500000000000000, -2.153805922287439945 ) ) ;
#1450 = DIRECTION ( 'NONE',  ( -0.02181900108494679719, 0.000000000000000000, 0.9997619372588931741 ) ) ;
#1451 = DATE_AND_TIME ( #8714, #9689 ) ;
#1452 = CARTESIAN_POINT ( 'NONE',  ( -67.62826500021935772, 13.12245405995659375, -201.7210169101921906 ) ) ;
#1453 = PLANE ( 'NONE',  #14090 ) ;
#1454 = ORIENTED_EDGE ( 'NONE', *, *, #7611, .F. ) ;
#1455 = CARTESIAN_POINT ( 'NONE',  ( 7.782455147742629364, 1.649526740344270381, 4.504548160689787473 ) ) ;
#1456 = CARTESIAN_POINT ( 'NONE',  ( -1.346194077712559167, 6.437500000000000888, -6.749999999999999112 ) ) ;
#1457 = CARTESIAN_POINT ( 'NONE',  ( -8.404493273108490925, 0.9205354583497085130, -105.1983221212521897 ) ) ;
#1458 = CARTESIAN_POINT ( 'NONE',  ( -2.298097038856278029, 0.6249999999999998890, -1.201902961143720638 ) ) ;
#1459 = CARTESIAN_POINT ( 'NONE',  ( 2.298097038856279362, 5.375000000000000888, -1.201902961143720860 ) ) ;
#1460 = CARTESIAN_POINT ( 'NONE',  ( -5.611193301459971750, 9.999999999999998224, -110.1737759617912786 ) ) ;
#1461 = LINE ( 'NONE', #2393, #4547 ) ;
#1462 = CARTESIAN_POINT ( 'NONE',  ( 8.807773658243950976, 15.00000000000000000, -105.8689255569521492 ) ) ;
#1463 = CARTESIAN_POINT ( 'NONE',  ( -3.980102097228897245E-16, 5.500000000000000000, -6.749999999999999112 ) ) ;
#1464 = CARTESIAN_POINT ( 'NONE',  ( -3.980102097228897738E-16, 15.00000000000000178, -6.749999999999999112 ) ) ;
#1465 = CARTESIAN_POINT ( 'NONE',  ( 3.749999999999999112, 6.687500000000000888, -5.053300858899108405 ) ) ;
#1466 = CARTESIAN_POINT ( 'NONE',  ( 3.749999999999999112, 8.187500000000000000, -5.053300858899108405 ) ) ;
#1467 = CARTESIAN_POINT ( 'NONE',  ( 2.538077654277008488, 14.29157444423261758, 1.114435963501728022 ) ) ;
#1468 = EDGE_CURVE ( 'NONE', #15191, #1027, #7393, .T. ) ;
#1469 = CARTESIAN_POINT ( 'NONE',  ( 12.97570930512322285, 3.737837276592360869, -166.4113073631658324 ) ) ;
#1470 = CARTESIAN_POINT ( 'NONE',  ( 4.507463604512255806, 5.000000000000000000, 2.585105772303601945 ) ) ;
#1471 = CARTESIAN_POINT ( 'NONE',  ( -24.86990227130816322, 5.000000000000000888, -145.8847246090277281 ) ) ;
#1472 = CARTESIAN_POINT ( 'NONE',  ( 0.7552767017137608230, 8.673617379884034486E-16, -110.7727649483667847 ) ) ;
#1473 = CARTESIAN_POINT ( 'NONE',  ( -4.979830621673884572, 8.673617379884032514E-16, -150.2731933682584327 ) ) ;
#1474 = CARTESIAN_POINT ( 'NONE',  ( 0.3766621274091721538, 0.3292059843107342232, -7.146945437571387671 ) ) ;
#1475 = EDGE_LOOP ( 'NONE', ( #14338, #13003, #3123, #7578 ) ) ;
#1476 = CC_DESIGN_APPROVAL ( #12728, ( #9370 ) ) ;
#1477 = CARTESIAN_POINT ( 'NONE',  ( -4.592425496802573972E-16, 8.000000000000000000, -7.250000000000000000 ) ) ;
#1478 = ORIENTED_EDGE ( 'NONE', *, *, #11230, .T. ) ;
#1479 = CARTESIAN_POINT ( 'NONE',  ( -3.431082444819314681, 4.336808689942017736E-16, -108.8148713286762046 ) ) ;
#1480 = CARTESIAN_POINT ( 'NONE',  ( -7.194037649453649763, 0.000000000000000000, -45.55632290616381397 ) ) ;
#1481 = CARTESIAN_POINT ( 'NONE',  ( 3.749999999999998668, 8.687500000000000000, -5.053300858899107517 ) ) ;
#1482 = CARTESIAN_POINT ( 'NONE',  ( 3.749999999999999112, 6.312500000000000000, -1.946699141100893149 ) ) ;
#1483 = VECTOR ( 'NONE', #11234, 1000.000000000000227 ) ;
#1484 = CC_DESIGN_PERSON_AND_ORGANIZATION_ASSIGNMENT ( #420, #4822, ( #10865 ) ) ;
#1485 = DIRECTION ( 'NONE',  ( -0.000000000000000000, -1.000000000000000000, -0.000000000000000000 ) ) ;
#1486 = EDGE_LOOP ( 'NONE', ( #897, #6728, #13316, #1428 ) ) ;
#1487 = CARTESIAN_POINT ( 'NONE',  ( 0.000000000000000000, 3.500000000000000000, -0.2500000000000002220 ) ) ;
#1488 = EDGE_CURVE ( 'NONE', #7451, #3391, #6082, .T. ) ;
#1489 = CARTESIAN_POINT ( 'NONE',  ( -1.553300858899107295, 11.43750000000000000, -7.250000000000000000 ) ) ;
#1490 = CARTESIAN_POINT ( 'NONE',  ( -68.53010506246435796, 15.00000000000343370, -179.3208756447880035 ) ) ;
#1491 = EDGE_CURVE ( 'NONE', #8920, #14065, #8555, .T. ) ;
#1492 = EDGE_CURVE ( 'NONE', #4560, #559, #12979, .T. ) ;
#1493 = APPROVAL_PERSON_ORGANIZATION ( #11249, #3278, #13730 ) ;
#1494 = CARTESIAN_POINT ( 'NONE',  ( 20.87131526946579285, 0.000000000000000000, -138.9752963459259547 ) ) ;
#1495 = DIRECTION ( 'NONE',  ( 0.000000000000000000, 0.000000000000000000, 1.000000000000000000 ) ) ;
#1496 = CARTESIAN_POINT ( 'NONE',  ( -3.980102097228897245E-16, 7.500000000000000000, -6.749999999999999112 ) ) ;
#1497 = VECTOR ( 'NONE', #9994, 1000.000000000000000 ) ;
#1498 = CARTESIAN_POINT ( 'NONE',  ( -7.159798564871144855, 9.999999999993500310, -124.1957246866965932 ) ) ;
#1499 = DATE_TIME_ROLE ( 'classification_date' ) ;
#1500 = CARTESIAN_POINT ( 'NONE',  ( -0.2690694657484744012, -4.336808689942017736E-15, -126.9559471811042499 ) ) ;
#1501 = LINE ( 'NONE', #1808, #1483 ) ;
#1502 = ORIENTED_EDGE ( 'NONE', *, *, #5053, .F. ) ;
#1503 = CARTESIAN_POINT ( 'NONE',  ( -0.3766621274091715987, 0.5000000000000000000, 0.1491815183709511716 ) ) ;
#1504 = CARTESIAN_POINT ( 'NONE',  ( -1.346194077712559167, 14.43750000000000000, -6.749999999999999112 ) ) ;
#1505 = ORIENTED_EDGE ( 'NONE', *, *, #365, .F. ) ;
#1506 = ORIENTED_EDGE ( 'NONE', *, *, #10462, .F. ) ;
#1507 = CARTESIAN_POINT ( 'NONE',  ( 26.04664898474823431, 2.285168050702167442, -138.3460210313947414 ) ) ;
#1508 = CARTESIAN_POINT ( 'NONE',  ( 3.749999999999999556, 14.25000000000000178, -3.500000000000000444 ) ) ;
#1509 = CARTESIAN_POINT ( 'NONE',  ( 2.298097038856278029, 11.12500000000000178, -5.798097038856279362 ) ) ;
#1510 = CARTESIAN_POINT ( 'NONE',  ( -3.249999999999999112, 10.68750000000000178, -2.153805922287440833 ) ) ;
#1511 = ORIENTED_EDGE ( 'NONE', *, *, #8371, .F. ) ;
#1512 = CIRCLE ( 'NONE', #14350, 5.000000000000002665 ) ;
#1513 = DIRECTION ( 'NONE',  ( 0.000000000000000000, 1.000000000000000000, 0.000000000000000000 ) ) ;
#1514 = CARTESIAN_POINT ( 'NONE',  ( -1.346194077712559389, 8.062500000000000000, -0.2500000000000002220 ) ) ;
#1515 = CIRCLE ( 'NONE', #3476, 6.000000000000002665 ) ;
#1516 = CARTESIAN_POINT ( 'NONE',  ( -9.240119717576693148, 2.330807083298499727, -104.6630069175297706 ) ) ;
#1517 = DIRECTION ( 'NONE',  ( -0.08794243244722436958, 0.000000000000000000, -0.9961255586397055328 ) ) ;
#1518 = CARTESIAN_POINT ( 'NONE',  ( -56.40225323527551637, 14.99999999999999645, -165.3314606177903272 ) ) ;
#1519 = PERSON_AND_ORGANIZATION_ROLE ( 'classification_officer' ) ;
#1520 = VECTOR ( 'NONE', #6716, 999.9999999999998863 ) ;
#1521 = B_SPLINE_CURVE_WITH_KNOTS ( 'NONE', 3,
 ( #14049, #3446, #8160, #11789, #3607, #5911, #8309, #8384, #13037, #11863 ),
 .UNSPECIFIED., .F., .F.,
 ( 4, 2, 2, 2, 4 ),
 ( 0.000000000000000000, 0.0007311508082448065502, 0.001462301616489612667, 0.002193452424734418892, 0.002924603232979224900 ),
 .UNSPECIFIED. ) ;
#1522 = CARTESIAN_POINT ( 'NONE',  ( -25.28756687824467164, 0.04309856747023026874, -200.8615385504288042 ) ) ;
#1523 = ORIENTED_EDGE ( 'NONE', *, *, #8090, .F. ) ;
#1524 = CARTESIAN_POINT ( 'NONE',  ( -1.346194077712559389, 2.437500000000000444, -6.749999999999999112 ) ) ;
#1525 = CARTESIAN_POINT ( 'NONE',  ( 2.651650429449553759, 11.87500000000000000, -0.8483495705504471296 ) ) ;
#1526 = CARTESIAN_POINT ( 'NONE',  ( -0.3766621274091715987, -0.2500000000000000000, -0.1347136637304948981 ) ) ;
#1527 = CARTESIAN_POINT ( 'NONE',  ( 2.651650429449552870, 15.12500000000000000, -6.151650429449553314 ) ) ;
#1528 = CARTESIAN_POINT ( 'NONE',  ( -67.60597199914535338, 11.34385781021491368, -204.0782660919513773 ) ) ;
#1529 = CARTESIAN_POINT ( 'NONE',  ( -0.2500000000000000555, 5.000000000000000000, -1.499999999999999778 ) ) ;
#1530 = CARTESIAN_POINT ( 'NONE',  ( 6.931531743086595476, 0.03088707369331828573, -105.1762940087775462 ) ) ;
#1531 = APPROVAL_DATE_TIME ( #1451, #8931 ) ;
#1532 = PRODUCT ( 'PruningShears_Predeterminado', 'PruningShears_Predeterminado', '', ( #4224 ) ) ;
#1533 = CARTESIAN_POINT ( 'NONE',  ( -67.58382170693636226, 10.00000000000000000, -204.5178482451963191 ) ) ;
#1534 = VERTEX_POINT ( 'NONE', #15310 ) ;
#1535 = CARTESIAN_POINT ( 'NONE',  ( 4.054307694666515971, 0.1412400999502742005, -0.4194500301308927148 ) ) ;
#1536 = CARTESIAN_POINT ( 'NONE',  ( -3.249999999999999556, 7.312500000000000000, -4.846194077712557835 ) ) ;
#1537 = EDGE_CURVE ( 'NONE', #13049, #10207, #3619, .T. ) ;
#1538 = CARTESIAN_POINT ( 'NONE',  ( -70.08363909706210393, 10.00000000000000178, -190.3084480996344894 ) ) ;
#1539 = CARTESIAN_POINT ( 'NONE',  ( -3.980102097228897245E-16, 14.50000000000000000, -6.749999999999999112 ) ) ;
#1540 = CARTESIAN_POINT ( 'NONE',  ( 2.298097038856279362, 9.374999999999998224, -1.201902961143720860 ) ) ;
#1541 = DIRECTION ( 'NONE',  ( 0.000000000000000000, -1.000000000000000000, -0.000000000000000000 ) ) ;
#1542 = CARTESIAN_POINT ( 'NONE',  ( 0.02975126090548325941, 2.500000000000000444, 0.3369930824702306316 ) ) ;
#1543 = B_SPLINE_CURVE_WITH_KNOTS ( 'NONE', 3,
 ( #10943, #12961, #2368, #8537, #5905, #10859 ),
 .UNSPECIFIED., .F., .F.,
 ( 4, 2, 4 ),
 ( 0.000000000000000000, 0.004544361750299368875, 0.009088723500598737751 ),
 .UNSPECIFIED. ) ;
#1544 = CARTESIAN_POINT ( 'NONE',  ( 10.96566884988558499, 13.79079921796280850, -106.3305639400367966 ) ) ;
#1545 = CARTESIAN_POINT ( 'NONE',  ( 3.249999999999999556, 5.750000000000000000, -3.500000000000000000 ) ) ;
#1546 = CARTESIAN_POINT ( 'NONE',  ( 3.749999999999999112, 1.312500000000000000, -1.946699141100893149 ) ) ;
#1547 = CARTESIAN_POINT ( 'NONE',  ( -4.592425496802573972E-16, 3.500000000000000000, -7.249999999999999112 ) ) ;
#1548 = CARTESIAN_POINT ( 'NONE',  ( -3.822630838043659995, 11.22863355747944070, -45.03847635001736904 ) ) ;
#1549 = CARTESIAN_POINT ( 'NONE',  ( -1.553300858899106629, 6.562500000000000888, 0.2500000000000002220 ) ) ;
#1550 = CARTESIAN_POINT ( 'NONE',  ( 3.873902325247619238, 13.05645226711805584, 3.961767634410926497 ) ) ;
#1551 = CARTESIAN_POINT ( 'NONE',  ( 4.329912723285513465, -2.075239479414269894, -43.25836301743400725 ) ) ;
#1552 = AXIS2_PLACEMENT_3D ( 'NONE', #7228, #9333, #4841 ) ;
#1553 = CARTESIAN_POINT ( 'NONE',  ( -8.469744009338400659, 7.499999999999991118, -95.93694702384601669 ) ) ;
#1554 = CARTESIAN_POINT ( 'NONE',  ( 1.167531179896777349, 3.999999999999993783, -139.4941991647475845 ) ) ;
#1555 = CARTESIAN_POINT ( 'NONE',  ( 0.000000000000000000, 15.00000000000000000, -0.2500000000000002220 ) ) ;
#1556 = CARTESIAN_POINT ( 'NONE',  ( -25.62073099797099829, 8.673617379884033500E-16, -189.4007417957344046 ) ) ;
#1557 = ORIENTED_EDGE ( 'NONE', *, *, #4888, .T. ) ;
#1558 = EDGE_CURVE ( 'NONE', #13993, #3117, #2467, .T. ) ;
#1559 = CARTESIAN_POINT ( 'NONE',  ( 0.000000000000000000, 14.50000000000000000, 0.2500000000000002220 ) ) ;
#1560 = EDGE_LOOP ( 'NONE', ( #3843, #13117, #4746, #11499 ) ) ;
#1561 = CARTESIAN_POINT ( 'NONE',  ( 26.15341798802279527, 4.000000000000000000, -138.7600702976168066 ) ) ;
#1562 = CARTESIAN_POINT ( 'NONE',  ( -25.04366442233794032, -1.809973046420242971E-12, -207.8080138893894002 ) ) ;
#1563 = CARTESIAN_POINT ( 'NONE',  ( -1.553300858899107295, 9.437500000000000000, -7.250000000000000000 ) ) ;
#1564 = CARTESIAN_POINT ( 'NONE',  ( -1.553300858899107073, 8.937500000000000000, -7.249999999999999112 ) ) ;
#1565 = CARTESIAN_POINT ( 'NONE',  ( 10.02369947906852232, 1.750000000002257083, 14.18264983478496966 ) ) ;
#1566 = EDGE_LOOP ( 'NONE', ( #14097, #9470, #2283, #12579 ) ) ;
#1567 = CARTESIAN_POINT ( 'NONE',  ( -9.192419678266688265, 3.588159064098102480, -115.4428990047103838 ) ) ;
#1568 = AXIS2_PLACEMENT_3D ( 'NONE', #4173, #11049, #8877 ) ;
#1569 = CARTESIAN_POINT ( 'NONE',  ( -2.298097038856279362, 3.875000000000000444, -5.798097038856278473 ) ) ;
#1570 = CARTESIAN_POINT ( 'NONE',  ( -3.750000000000000000, 9.250000000000000000, -3.499999999999999112 ) ) ;
#1571 = CARTESIAN_POINT ( 'NONE',  ( -68.53010506257494683, 9.999999999999998224, -179.3208756447420171 ) ) ;
#1572 = CARTESIAN_POINT ( 'NONE',  ( 2.850044070969222521, 9.999999999999998224, -103.0233998225063345 ) ) ;
#1573 = CARTESIAN_POINT ( 'NONE',  ( -3.249999999999999556, 7.187500000000000000, -2.153805922287440833 ) ) ;
#1574 = DIRECTION ( 'NONE',  ( 0.000000000000000000, 1.000000000000000000, 0.000000000000000000 ) ) ;
#1575 = APPROVAL_ROLE ( '' ) ;
#1576 = CARTESIAN_POINT ( 'NONE',  ( -8.651617673122958152, 5.000000000001580069, -120.1343837246376580 ) ) ;
#1577 = CARTESIAN_POINT ( 'NONE',  ( 8.348030713529086100, 5.000000000000000888, -112.8139498890671746 ) ) ;
#1578 = VERTEX_POINT ( 'NONE', #213 ) ;
#1579 = CIRCLE ( 'NONE', #6519, 3.500000000000000000 ) ;
#1580 = LINE ( 'NONE', #424, #5918 ) ;
#1581 = VECTOR ( 'NONE', #3087, 1000.000000000000114 ) ;
#1582 = DIRECTION ( 'NONE',  ( 0.02181900108494732801, 0.000000000000000000, -0.9997619372588932851 ) ) ;
#1583 = EDGE_LOOP ( 'NONE', ( #14859, #10275 ) ) ;
#1584 = EDGE_CURVE ( 'NONE', #7183, #12677, #2616, .T. ) ;
#1585 = EDGE_LOOP ( 'NONE', ( #9449, #3500 ) ) ;
#1586 = DIRECTION ( 'NONE',  ( 0.08794243244723003172, 0.000000000000000000, 0.9961255586397049777 ) ) ;
#1587 = CARTESIAN_POINT ( 'NONE',  ( -1.553300858899106629, 11.56250000000000178, 0.2499999999999998335 ) ) ;
#1588 = CARTESIAN_POINT ( 'NONE',  ( -1.346194077712559167, 9.937500000000001776, -6.749999999999999112 ) ) ;
#1589 = EDGE_CURVE ( 'NONE', #6397, #10866, #6683, .T. ) ;
#1590 = CARTESIAN_POINT ( 'NONE',  ( -2.298097038856279362, 10.87499999999999822, -5.798097038856278473 ) ) ;
#1591 = EDGE_LOOP ( 'NONE', ( #6786, #11330, #11607, #12722, #9213, #14506 ) ) ;
#1592 = CARTESIAN_POINT ( 'NONE',  ( -63.21422130130007133, 5.000000000000000000, -203.6040552426024703 ) ) ;
#1593 = CARTESIAN_POINT ( 'NONE',  ( -2.298097038856278473, 6.125000000000000000, -1.201902961143720416 ) ) ;
#1594 = AXIS2_PLACEMENT_3D ( 'NONE', #11291, #713, #5417 ) ;
#1595 = CARTESIAN_POINT ( 'NONE',  ( 12.80672841695803577, 14.26859485420106211, -125.9388545821283003 ) ) ;
#1596 = CARTESIAN_POINT ( 'NONE',  ( -54.80198710092766134, 10.00000000000000000, -172.3578233953475376 ) ) ;
#1597 = DIRECTION ( 'NONE',  ( 0.000000000000000000, 0.000000000000000000, 1.000000000000000000 ) ) ;
#1598 = APPROVAL_ROLE ( '' ) ;
#1599 = CARTESIAN_POINT ( 'NONE',  ( 0.4711736884522539359, 15.00000000000000000, 5.336993082470237404 ) ) ;
#1600 = EDGE_LOOP ( 'NONE', ( #5553, #7505, #12230, #10621, #169 ) ) ;
#1601 = CARTESIAN_POINT ( 'NONE',  ( -3.980102097228897245E-16, 1.500000000000000000, -6.749999999999999112 ) ) ;
#1602 = AXIS2_PLACEMENT_3D ( 'NONE', #8066, #14029, #3425 ) ;
#1603 = CARTESIAN_POINT ( 'NONE',  ( -2.651650429449553314, 13.37500000000000000, -6.151650429449552426 ) ) ;
#1604 = EDGE_CURVE ( 'NONE', #1578, #13029, #5211, .T. ) ;
#1605 = VERTEX_POINT ( 'NONE', #2774 ) ;
#1606 = CARTESIAN_POINT ( 'NONE',  ( -6.807027589832401304, 1.750000000000027311, 11.03434205495325848 ) ) ;
#1607 = CARTESIAN_POINT ( 'NONE',  ( -3.750000000000000000, 2.250000000000000444, -3.499999999999999112 ) ) ;
#1608 = CARTESIAN_POINT ( 'NONE',  ( -65.16270098009177048, 15.39946212108827162, -205.5516834495680598 ) ) ;
#1609 = LINE ( 'NONE', #13208, #537 ) ;
#1610 = CARTESIAN_POINT ( 'NONE',  ( -1.553300858899107073, 1.437500000000000000, -7.250000000000000000 ) ) ;
#1611 = PERSON_AND_ORGANIZATION_ROLE ( 'creator' ) ;
#1612 = CARTESIAN_POINT ( 'NONE',  ( -67.59204273365905635, 13.51751734435156393, -200.6893734332653310 ) ) ;
#1613 = CARTESIAN_POINT ( 'NONE',  ( 9.933893833910557802, 12.49999999999999822, -126.1398084322751885 ) ) ;
#1614 = ORIENTED_EDGE ( 'NONE', *, *, #3097, .T. ) ;
#1615 = CARTESIAN_POINT ( 'NONE',  ( 26.65632903789428099, 4.223198481467347776, -136.8991823062413857 ) ) ;
#1616 = CARTESIAN_POINT ( 'NONE',  ( 3.249999999999999112, 5.812500000000000000, -2.153805922287439945 ) ) ;
#1617 = CARTESIAN_POINT ( 'NONE',  ( -52.57969357448924796, 9.999999999999998224, -146.7268407086697550 ) ) ;
#1618 = CARTESIAN_POINT ( 'NONE',  ( 1.346194077712558057, 14.56250000000000000, -6.750000000000000000 ) ) ;
#1619 = CARTESIAN_POINT ( 'NONE',  ( 3.249999999999999556, 10.25000000000000178, -3.500000000000000000 ) ) ;
#1620 = CARTESIAN_POINT ( 'NONE',  ( -0.4873557683217199510, 10.00000000000000000, -103.5659326153046038 ) ) ;
#1621 = CYLINDRICAL_SURFACE ( 'NONE', #12187, 5.000000000000000000 ) ;
#1622 = CARTESIAN_POINT ( 'NONE',  ( -25.68053481550299111, 15.00000000000000000, -142.4798935003980773 ) ) ;
#1623 = CARTESIAN_POINT ( 'NONE',  ( 1.346194077712560944, 2.937500000000000444, -0.2500000000000010547 ) ) ;
#1624 = CARTESIAN_POINT ( 'NONE',  ( -1.553300858899106629, 5.562500000000000000, 0.2499999999999998335 ) ) ;
#1625 = CARTESIAN_POINT ( 'NONE',  ( 3.750000000000000000, 8.750000000000000000, -3.500000000000000444 ) ) ;
#1626 = CARTESIAN_POINT ( 'NONE',  ( -3.911481695397140079, 10.31382935203035700, -44.10643064657414669 ) ) ;
#1627 = CARTESIAN_POINT ( 'NONE',  ( -2.651650429449553314, 4.875000000000000000, -6.151650429449552426 ) ) ;
#1628 = CARTESIAN_POINT ( 'NONE',  ( 4.999999999999998224, 1.301042606982605321E-15, -45.97309604003012140 ) ) ;
#1629 = DIRECTION ( 'NONE',  ( -1.000000000000000000, -0.000000000000000000, -0.000000000000000000 ) ) ;
#1630 = LINE ( 'NONE', #5190, #11951 ) ;
#1631 = CARTESIAN_POINT ( 'NONE',  ( 5.570677809474934072, 7.976916236371252995E-16, -141.9062416701571863 ) ) ;
#1632 = CARTESIAN_POINT ( 'NONE',  ( -25.59460798226730915, 8.673617379884035472E-16, -196.2441450656505992 ) ) ;
#1633 = EDGE_LOOP ( 'NONE', ( #13335, #9291, #5814, #15267, #5455, #6069 ) ) ;
#1634 = CARTESIAN_POINT ( 'NONE',  ( 0.000000000000000000, -0.4999999999999999445, -0.2500000000000002220 ) ) ;
#1635 = ORIENTED_EDGE ( 'NONE', *, *, #14289, .F. ) ;
#1636 = CARTESIAN_POINT ( 'NONE',  ( 0.3766621274091715987, 0.5000000000000000000, -0.1347136637304948981 ) ) ;
#1637 = CARTESIAN_POINT ( 'NONE',  ( -23.81014751474988245, 4.000000000000494715, -207.0536590050782593 ) ) ;
#1638 = CARTESIAN_POINT ( 'NONE',  ( -3.750000000000000000, 10.25000000000000000, -3.499999999999999112 ) ) ;
#1639 = CARTESIAN_POINT ( 'NONE',  ( -3.750000000000000000, 8.687500000000003553, -1.946699141100893149 ) ) ;
#1640 = CARTESIAN_POINT ( 'NONE',  ( 26.28048204801264731, 0.000000000000000000, 69.48733826436532013 ) ) ;
#1641 = ORIENTED_EDGE ( 'NONE', *, *, #6101, .F. ) ;
#1642 = CARTESIAN_POINT ( 'NONE',  ( -9.345007083233795697, 4.277268689418242786, -115.3736373665757498 ) ) ;
#1643 = CARTESIAN_POINT ( 'NONE',  ( -3.249999999999999556, 3.750000000000000444, -3.500000000000000000 ) ) ;
#1644 = EDGE_CURVE ( 'NONE', #8227, #14065, #14, .T. ) ;
#1645 = CARTESIAN_POINT ( 'NONE',  ( -2.651650429449553314, 11.37500000000000000, -6.151650429449552426 ) ) ;
#1646 = CARTESIAN_POINT ( 'NONE',  ( -70.10710660171159248, 9.999999999999998224, -192.1972859456682272 ) ) ;
#1647 = ADVANCED_FACE ( 'NONE', ( #13601 ), #15162, .F. ) ;
#1648 = DATE_AND_TIME ( #13558, #3508 ) ;
#1649 = CARTESIAN_POINT ( 'NONE',  ( 3.249999999999999556, 8.750000000000000000, -3.500000000000000000 ) ) ;
#1650 = CARTESIAN_POINT ( 'NONE',  ( -1.724164254788412842, 5.321094445766560987, -19.52964039877223712 ) ) ;
#1651 = CARTESIAN_POINT ( 'NONE',  ( -9.756303285186648466, 5.000000000000004441, -116.2179163664056176 ) ) ;
#1652 = CARTESIAN_POINT ( 'NONE',  ( 8.346107330820501602, 5.000000000000000888, -114.8449120967954116 ) ) ;
#1653 = CARTESIAN_POINT ( 'NONE',  ( -0.3766621274091715987, -0.2500000000000000000, -7.146945437571387671 ) ) ;
#1654 = DIRECTION ( 'NONE',  ( 0.000000000000000000, 1.000000000000000000, -0.000000000000000000 ) ) ;
#1655 = ORIENTED_EDGE ( 'NONE', *, *, #14828, .T. ) ;
#1656 = CARTESIAN_POINT ( 'NONE',  ( 10.99340860758278460, 5.943472311793079221, -45.60560901953395785 ) ) ;
#1657 = CARTESIAN_POINT ( 'NONE',  ( 0.000000000000000000, 0.000000000000000000, 0.000000000000000000 ) ) ;
#1658 = CARTESIAN_POINT ( 'NONE',  ( 3.749999999999999112, 11.31250000000000355, -1.946699141100893149 ) ) ;
#1659 = CARTESIAN_POINT ( 'NONE',  ( 0.000000000000000000, 10.50000000000000000, -0.2500000000000002220 ) ) ;
#1660 = CARTESIAN_POINT ( 'NONE',  ( 3.249999999999998224, 13.18750000000000000, -4.846194077712561388 ) ) ;
#1661 = EDGE_LOOP ( 'NONE', ( #5589, #1980, #6842, #9673 ) ) ;
#1662 = CLOSED_SHELL ( 'NONE', ( #7737, #15014, #7787, #3243, #13011, #13938, #9045, #14931, #2350, #1864, #9390, #10283, #3651, #15291, #11753, #4537, #13090, #449, #10997, #58, #13744, #5453, #13226, #15012, #3092, #6226, #1730, #3438, #8060, #8777, #2977, #13473, #11933, #4422, #6588, #3630, #13410, #5924, #9781, #9302, #9383, #13206, #3954, #2049, #9694, #8178, #4869, #4115, #3265, #7713, #8567, #13066, #11586, #3270, #4200, #818, #9047, #13191, #6344, #3477, #14846, #7870, #13411, #9664, #8565, #1943, #13205, #252, #6858, #4238, #10365, #14316, #8728, #6312, #5991, #7625, #6166, #12049, #12321 ) ) ;
#1663 = CARTESIAN_POINT ( 'NONE',  ( 1.346194077712558057, 6.562500000000000000, -6.750000000000000000 ) ) ;
#1664 = FACE_OUTER_BOUND ( 'NONE', #3413, .T. ) ;
#1665 = APPLICATION_CONTEXT ( 'configuration controlled 3d designs of mechanical parts and assemblies' ) ;
#1666 = CARTESIAN_POINT ( 'NONE',  ( 1.114947364559086829, 5.000000000000000888, -139.4079432275550232 ) ) ;
#1667 = CARTESIAN_POINT ( 'NONE',  ( 0.000000000000000000, 1.750000000000000000, 0.000000000000000000 ) ) ;
#1668 = EDGE_CURVE ( 'NONE', #8206, #10375, #1993, .T. ) ;
#1669 = COORDINATED_UNIVERSAL_TIME_OFFSET ( 0, 0, .AHEAD. ) ;
#1670 = CARTESIAN_POINT ( 'NONE',  ( -24.82846637880105334, 2.415521945931450976, -207.8856318682263407 ) ) ;
#1671 = EDGE_LOOP ( 'NONE', ( #9331, #1047, #5629, #2198, #8005 ) ) ;
#1672 = CARTESIAN_POINT ( 'NONE',  ( -1.346194077712559389, 0.4375000000000000555, -6.749999999999999112 ) ) ;
#1673 = CARTESIAN_POINT ( 'NONE',  ( 0.000000000000000000, -0.4999999999999999445, 0.2500000000000002220 ) ) ;
#1674 = VERTEX_POINT ( 'NONE', #6247 ) ;
#1675 = DIRECTION ( 'NONE',  ( -0.02181900108494707127, 0.000000000000000000, 0.9997619372588930631 ) ) ;
#1676 = CARTESIAN_POINT ( 'NONE',  ( -3.749999999999999556, 1.187500000000000444, -1.946699141100892927 ) ) ;
#1677 = CARTESIAN_POINT ( 'NONE',  ( 11.04730217088350663, 5.000000000000000888, -107.1178495010082941 ) ) ;
#1678 = EDGE_CURVE ( 'NONE', #3245, #11140, #14355, .T. ) ;
#1679 = CARTESIAN_POINT ( 'NONE',  ( 0.4757783475439041343, 3.128924928913413339, 5.389150141154763318 ) ) ;
#1680 = CARTESIAN_POINT ( 'NONE',  ( -3.750000000000000000, 2.250000000000000444, -3.499999999999999112 ) ) ;
#1681 = EDGE_CURVE ( 'NONE', #9756, #1124, #614, .T. ) ;
#1682 = DATE_AND_TIME ( #9802, #10426 ) ;
#1683 = EDGE_CURVE ( 'NONE', #6835, #914, #2487, .T. ) ;
#1684 = CARTESIAN_POINT ( 'NONE',  ( -67.61802425151131501, 11.74280943683806377, -203.7724845797763464 ) ) ;
#1685 = DIRECTION ( 'NONE',  ( 0.000000000000000000, 0.000000000000000000, 1.000000000000000000 ) ) ;
#1686 = EDGE_LOOP ( 'NONE', ( #14143, #6792, #4267, #8751 ) ) ;
#1687 = CARTESIAN_POINT ( 'NONE',  ( -3.249999999999999556, 6.312500000000000000, -4.846194077712557835 ) ) ;
#1688 = CARTESIAN_POINT ( 'NONE',  ( -32.47904071408094495, 15.00000000000000000, -151.1158311594353734 ) ) ;
#1689 = CARTESIAN_POINT ( 'NONE',  ( -3.249999999999999556, 13.31250000000000000, -4.846194077712557835 ) ) ;
#1690 = CARTESIAN_POINT ( 'NONE',  ( -1.346194077712558945, 12.56250000000000355, -0.2500000000000002220 ) ) ;
#1691 = CARTESIAN_POINT ( 'NONE',  ( 2.752881441477225355, 9.999999999999998224, 2.754251355355159081 ) ) ;
#1692 = CARTESIAN_POINT ( 'NONE',  ( -12.27209645382209757, 2.500000000000000444, -127.2227734861304782 ) ) ;
#1693 = CARTESIAN_POINT ( 'NONE',  ( 0.000000000000000000, 3.000000000000000000, -0.2500000000000002220 ) ) ;
#1694 = CARTESIAN_POINT ( 'NONE',  ( -4.592425496802573972E-16, 5.000000000000000000, -7.250000000000000000 ) ) ;
#1695 = CARTESIAN_POINT ( 'NONE',  ( 2.651650429449553759, 10.87500000000000178, -0.8483495705504471296 ) ) ;
#1696 = CARTESIAN_POINT ( 'NONE',  ( -5.836146573691881834, 0.2317559567678120491, -116.8702851668251128 ) ) ;
#1697 = CARTESIAN_POINT ( 'NONE',  ( -4.222591397270751834, 9.819471330552410393, -47.66802519420133422 ) ) ;
#1698 = CARTESIAN_POINT ( 'NONE',  ( 3.749999999999999556, 10.25000000000000178, -3.500000000000000444 ) ) ;
#1699 = CARTESIAN_POINT ( 'NONE',  ( 0.000000000000000000, 5.000000000000000000, 0.000000000000000000 ) ) ;
#1700 = CARTESIAN_POINT ( 'NONE',  ( 11.76219408996538895, 1.269473348720391082, -165.4091314653759639 ) ) ;
#1701 = CARTESIAN_POINT ( 'NONE',  ( 6.288457687488933523, 0.000000000000000000, -105.0111312234435985 ) ) ;
#1702 = CARTESIAN_POINT ( 'NONE',  ( -22.26570164085059389, 8.673617379884035472E-16, -175.9421475886515509 ) ) ;
#1703 = CARTESIAN_POINT ( 'NONE',  ( 6.049910241306248437, 0.000000000000000000, -118.3734240199295300 ) ) ;
#1704 = DESIGN_CONTEXT ( 'detailed design', #5805, 'design' ) ;
#1705 = CARTESIAN_POINT ( 'NONE',  ( 8.125871712912910994, 2.250174624375246513, 2.357012527964847948 ) ) ;
#1706 = CARTESIAN_POINT ( 'NONE',  ( 3.750000000000000000, 12.31250000000000178, -1.946699141100892705 ) ) ;
#1707 = ORIENTED_EDGE ( 'NONE', *, *, #10438, .F. ) ;
#1708 = CARTESIAN_POINT ( 'NONE',  ( 4.373577830794676657, 12.45268385026016666, -1.811168651986067468 ) ) ;
#1709 = DIRECTION ( 'NONE',  ( -0.9961255586397055328, 0.000000000000000000, 0.08794243244722428632 ) ) ;
#1710 = CARTESIAN_POINT ( 'NONE',  ( -3.749999999999999556, 10.18750000000000000, -1.946699141100892927 ) ) ;
#1711 = CARTESIAN_POINT ( 'NONE',  ( -1.553300858899107073, 7.937500000000001776, -7.249999999999999112 ) ) ;
#1712 = CARTESIAN_POINT ( 'NONE',  ( 26.88777289245747326, 5.000000000000000888, -138.4814624290440577 ) ) ;
#1713 = CARTESIAN_POINT ( 'NONE',  ( -8.888107754931237281, 2.324435220146938708, -116.5586263778049982 ) ) ;
#1714 = CARTESIAN_POINT ( 'NONE',  ( 3.249999999999998224, 9.187500000000001776, -4.846194077712561388 ) ) ;
#1715 = CARTESIAN_POINT ( 'NONE',  ( -3.750000000000000000, 14.25000000000000000, -3.499999999999999112 ) ) ;
#1716 = CARTESIAN_POINT ( 'NONE',  ( 1.893911505664648054, 0.000000000000000000, -1.663006917529762152 ) ) ;
#1717 = CARTESIAN_POINT ( 'NONE',  ( 2.678407845566782353, 1.921202954650393924, -1.000000000000027311 ) ) ;
#1718 = CALENDAR_DATE ( 2026, 8, 10 ) ;
#1719 = CARTESIAN_POINT ( 'NONE',  ( -1.346194077712559389, 12.06250000000000000, -0.2500000000000002220 ) ) ;
#1720 = CARTESIAN_POINT ( 'NONE',  ( -6.226828414324827143, 9.999999999999996447, -108.7107943239692673 ) ) ;
#1721 = LOCAL_TIME ( 12, 28, 20.00000000000000000, #2602 ) ;
#1722 = LINE ( 'NONE', #7673, #7012 ) ;
#1723 = CARTESIAN_POINT ( 'NONE',  ( 8.481465556250880056, -2.145889335582468041E-13, -115.9036014638424632 ) ) ;
#1724 = AXIS2_PLACEMENT_3D ( 'NONE', #2035, #11460, #880 ) ;
#1725 = LINE ( 'NONE', #8765, #10142 ) ;
#1726 = DIRECTION ( 'NONE',  ( 0.000000000000000000, 1.000000000000000000, 0.000000000000000000 ) ) ;
#1727 = ORIENTED_EDGE ( 'NONE', *, *, #1492, .F. ) ;
#1728 = EDGE_CURVE ( 'NONE', #11635, #4915, #9804, .T. ) ;
#1729 = VECTOR ( 'NONE', #14064, 1000.000000000000000 ) ;
#1730 = ADVANCED_FACE ( 'NONE', ( #9878, #7478 ), #12275, .F. ) ;
#1731 = CARTESIAN_POINT ( 'NONE',  ( -1.330285697047033366, 7.379999999999995453, -43.49585833228641008 ) ) ;
#1732 = CARTESIAN_POINT ( 'NONE',  ( 12.01748009419283925, 2.331468351711883680E-16, 57.58516622398010298 ) ) ;
#1733 = CARTESIAN_POINT ( 'NONE',  ( 1.553300858899109071, 11.43750000000000178, 0.2499999999999989175 ) ) ;
#1734 = CARTESIAN_POINT ( 'NONE',  ( 3.249999999999998224, 12.18750000000000178, -4.846194077712561388 ) ) ;
#1735 = CARTESIAN_POINT ( 'NONE',  ( -2.298097038856278029, 12.62500000000000000, -1.201902961143720638 ) ) ;
#1736 = EDGE_LOOP ( 'NONE', ( #13514, #5414, #2878, #5216 ) ) ;
#1737 = CARTESIAN_POINT ( 'NONE',  ( 0.000000000000000000, 13.00000000000000178, -0.2500000000000002220 ) ) ;
#1738 = CC_DESIGN_APPROVAL ( #3558, ( #9134 ) ) ;
#1739 = AXIS2_PLACEMENT_3D ( 'NONE', #6430, #872, #7587 ) ;
#1740 = FACE_OUTER_BOUND ( 'NONE', #8505, .T. ) ;
#1741 = CIRCLE ( 'NONE', #6426, 2.000000000000001776 ) ;
#1742 = CARTESIAN_POINT ( 'NONE',  ( -4.743345422599378303, 15.00000000000000000, -103.3611366015581154 ) ) ;
#1743 = CARTESIAN_POINT ( 'NONE',  ( 4.132056102115797991, 0.2279355446411715780, 0.3862057507398425349 ) ) ;
#1744 = CARTESIAN_POINT ( 'NONE',  ( -4.907357056059624689, 15.00000000000000000, -117.3740583286203076 ) ) ;
#1745 = CALENDAR_DATE ( 2026, 8, 10 ) ;
#1746 = DIRECTION ( 'NONE',  ( 0.000000000000000000, -1.000000000000000000, 0.000000000000000000 ) ) ;
#1747 = AXIS2_PLACEMENT_3D ( 'NONE', #1503, #9773, #13259 ) ;
#1748 = VERTEX_POINT ( 'NONE', #3004 ) ;
#1749 = CARTESIAN_POINT ( 'NONE',  ( -3.249999999999999556, 5.250000000000000000, -3.499999999999999556 ) ) ;
#1750 = CARTESIAN_POINT ( 'NONE',  ( 3.749999999999999112, 13.81250000000000000, -1.946699141100892039 ) ) ;
#1751 = VECTOR ( 'NONE', #780, 1000.000000000000114 ) ;
#1752 = TOROIDAL_SURFACE ( 'NONE', #1009, 9.800000000000245848, 5.000000000000000000 ) ;
#1753 = ORIENTED_EDGE ( 'NONE', *, *, #13116, .F. ) ;
#1754 = ADVANCED_FACE ( 'NONE', ( #9954 ), #14844, .T. ) ;
#1755 = CARTESIAN_POINT ( 'NONE',  ( 3.230086961373112242, 15.00000000000000000, 5.208283729180106292 ) ) ;
#1756 = CARTESIAN_POINT ( 'NONE',  ( 3.749999999999998668, 0.6875000000000000000, -5.053300858899107517 ) ) ;
#1757 = AXIS2_PLACEMENT_3D ( 'NONE', #9874, #2688, #378 ) ;
#1758 = CARTESIAN_POINT ( 'NONE',  ( 8.895558325401111688, 15.00000000000000000, -141.4560052469132643 ) ) ;
#1759 = CARTESIAN_POINT ( 'NONE',  ( 2.928550336651898789, 0.6497958086621815621, 2.702460884016614440 ) ) ;
#1760 = APPROVAL_ROLE ( '' ) ;
#1761 = CC_DESIGN_PERSON_AND_ORGANIZATION_ASSIGNMENT ( #9790, #283, ( #12090 ) ) ;
#1762 = DIRECTION ( 'NONE',  ( 0.000000000000000000, 1.000000000000000000, 0.000000000000000000 ) ) ;
#1763 = DIRECTION ( 'NONE',  ( -0.000000000000000000, -1.000000000000000000, -0.000000000000000000 ) ) ;
#1764 = VERTEX_POINT ( 'NONE', #14616 ) ;
#1765 = CARTESIAN_POINT ( 'NONE',  ( -2.298097038856278918, 10.37500000000000000, -5.798097038856277585 ) ) ;
#1766 = CARTESIAN_POINT ( 'NONE',  ( -69.76017711480231753, 9.999999999999998224, -197.5794603834288239 ) ) ;
#1767 = CARTESIAN_POINT ( 'NONE',  ( 3.249999999999998224, 3.312500000000000000, -2.153805922287439945 ) ) ;
#1768 =( GEOMETRIC_REPRESENTATION_CONTEXT ( 3 ) GLOBAL_UNCERTAINTY_ASSIGNED_CONTEXT ( ( #14226 ) ) GLOBAL_UNIT_ASSIGNED_CONTEXT ( ( #5521, #4369, #6899 ) ) REPRESENTATION_CONTEXT ( 'NONE', 'WORKASPACE' ) );
#1769 = CARTESIAN_POINT ( 'NONE',  ( -3.249999999999999556, 12.74999999999999822, -3.500000000000000000 ) ) ;
#1770 = LINE ( 'NONE', #12204, #2053 ) ;
#1771 = EDGE_CURVE ( 'NONE', #4454, #8744, #5444, .T. ) ;
#1772 = ADVANCED_FACE ( 'NONE', ( #11109 ), #8869, .T. ) ;
#1773 = CARTESIAN_POINT ( 'NONE',  ( -63.21422130130007133, 15.00000000000000000, -203.6040552426024703 ) ) ;
#1774 = CARTESIAN_POINT ( 'NONE',  ( -3.249999999999999556, 3.187500000000000000, -2.153805922287440833 ) ) ;
#1775 = CARTESIAN_POINT ( 'NONE',  ( 2.651650429449553314, 5.375000000000000000, -0.8483495705504476847 ) ) ;
#1776 = CARTESIAN_POINT ( 'NONE',  ( -3.750000000000000000, 11.31249999999999822, -5.053300858899105741 ) ) ;
#1777 = CARTESIAN_POINT ( 'NONE',  ( -17.32624372123753886, 2.500000000000000444, -122.3796757791585321 ) ) ;
#1778 = CARTESIAN_POINT ( 'NONE',  ( -3.329332828452641113, 9.806810919949601413, -43.39695214296718717 ) ) ;
#1779 = CC_DESIGN_PERSON_AND_ORGANIZATION_ASSIGNMENT ( #13490, #7949, ( #6227 ) ) ;
#1780 = CARTESIAN_POINT ( 'NONE',  ( -1.553300858899107073, 9.937500000000001776, -7.249999999999999112 ) ) ;
#1781 = CARTESIAN_POINT ( 'NONE',  ( 0.000000000000000000, 0.000000000000000000, -3.500000000000000000 ) ) ;
#1782 = APPROVAL_PERSON_ORGANIZATION ( #14841, #2516, #1760 ) ;
#1783 = CARTESIAN_POINT ( 'NONE',  ( 11.20997547022881058, 0.7546953127386059057, -164.9537947295017943 ) ) ;
#1784 = CARTESIAN_POINT ( 'NONE',  ( 23.10845500747044667, 2.100000000000000089, 28.62577620913018706 ) ) ;
#1785 = CARTESIAN_POINT ( 'NONE',  ( -26.07384356158112126, 3.269528285336324855E-12, -174.4700131545309603 ) ) ;
#1786 = DIRECTION ( 'NONE',  ( -0.000000000000000000, -1.000000000000000000, -0.000000000000000000 ) ) ;
#1787 = CARTESIAN_POINT ( 'NONE',  ( -36.05823818790233304, 15.00000000000000000, -151.2682901559026334 ) ) ;
#1788 = CARTESIAN_POINT ( 'NONE',  ( 0.000000000000000000, 12.50000000000000178, 0.2500000000000002220 ) ) ;
#1789 = ORIENTED_EDGE ( 'NONE', *, *, #9515, .F. ) ;
#1790 = PLANE ( 'NONE',  #15147 ) ;
#1791 = CARTESIAN_POINT ( 'NONE',  ( 10.79258363242540497, 2.747348697280918461, -106.2503091257652699 ) ) ;
#1792 = CARTESIAN_POINT ( 'NONE',  ( -2.651650429449552870, 6.625000000000000000, -0.8483495705504467965 ) ) ;
#1793 = EDGE_CURVE ( 'NONE', #4876, #14091, #11126, .T. ) ;
#1794 = CARTESIAN_POINT ( 'NONE',  ( 26.13050938914192756, 6.000000000000000000, -138.2605953772281566 ) ) ;
#1795 = LOCAL_TIME ( 12, 28, 20.00000000000000000, #2070 ) ;
#1796 = CC_DESIGN_PERSON_AND_ORGANIZATION_ASSIGNMENT ( #5768, #9477, ( #11824 ) ) ;
#1797 = CARTESIAN_POINT ( 'NONE',  ( -9.131312970616235702, 2.485997537948267944, -116.0049100415185137 ) ) ;
#1798 = CARTESIAN_POINT ( 'NONE',  ( -2.298097038856278029, 6.625000000000000000, -1.201902961143720638 ) ) ;
#1799 = DIRECTION ( 'NONE',  ( 0.000000000000000000, 0.000000000000000000, -1.000000000000000000 ) ) ;
#1800 = CARTESIAN_POINT ( 'NONE',  ( -3.749999999999999556, 12.18750000000000000, -1.946699141100892927 ) ) ;
#1801 = AXIS2_PLACEMENT_3D ( 'NONE', #14947, #9050, #13999 ) ;
#1802 = CARTESIAN_POINT ( 'NONE',  ( -67.29661116483784156, 9.999999999999998224, -205.0278900928575183 ) ) ;
#1803 = CARTESIAN_POINT ( 'NONE',  ( -8.289881740238502772, -2.075239479414269894, -35.21986562831451550 ) ) ;
#1804 = PERSON_AND_ORGANIZATION ( #3176, #3020 ) ;
#1805 = CARTESIAN_POINT ( 'NONE',  ( 2.298097038856279362, 11.87500000000000000, -1.201902961143720860 ) ) ;
#1806 = CARTESIAN_POINT ( 'NONE',  ( 4.329912723285513465, 2.075239479414269894, -43.25836301743400725 ) ) ;
#1807 = DIRECTION ( 'NONE',  ( -0.000000000000000000, -1.000000000000000000, -0.000000000000000000 ) ) ;
#1808 = CARTESIAN_POINT ( 'NONE',  ( 0.4711736884522539359, 9.999999999999998224, 5.336993082470237404 ) ) ;
#1809 = CARTESIAN_POINT ( 'NONE',  ( 2.011321487292375032, 9.999999999999998224, -137.8771695030452520 ) ) ;
#1810 = CARTESIAN_POINT ( 'NONE',  ( 0.000000000000000000, 3.061616997868383018E-17, -0.1347136637304948981 ) ) ;
#1811 = ORIENTED_EDGE ( 'NONE', *, *, #451, .T. ) ;
#1812 = CARTESIAN_POINT ( 'NONE',  ( 10.01029310660177529, 5.834492850526031837, -45.31678212580880682 ) ) ;
#1813 = LINE ( 'NONE', #6600, #9229 ) ;
#1814 = CARTESIAN_POINT ( 'NONE',  ( -2.651650429449552870, 2.125000000000000000, -0.8483495705504462414 ) ) ;
#1815 = CIRCLE ( 'NONE', #11424, 2.500000000000000000 ) ;
#1816 = CARTESIAN_POINT ( 'NONE',  ( -3.249999999999999556, 9.750000000000000000, -3.500000000000000000 ) ) ;
#1817 = CARTESIAN_POINT ( 'NONE',  ( -2.298097038856278918, 0.3750000000000000000, -5.798097038856277585 ) ) ;
#1818 = ORIENTED_EDGE ( 'NONE', *, *, #14993, .F. ) ;
#1819 = CARTESIAN_POINT ( 'NONE',  ( -1.346194077712559389, 10.43750000000000000, -6.749999999999999112 ) ) ;
#1820 = B_SPLINE_CURVE_WITH_KNOTS ( 'NONE', 3,
 ( #14626, #13609, #13380, #8804 ),
 .UNSPECIFIED., .F., .F.,
 ( 4, 4 ),
 ( 7.151554039766124246E-07, 0.0004291502618545642322 ),
 .UNSPECIFIED. ) ;
#1821 = CARTESIAN_POINT ( 'NONE',  ( 6.369258321017759350, -2.075239479414269894, -34.56909192082981974 ) ) ;
#1822 = CARTESIAN_POINT ( 'NONE',  ( 11.89832029942966152, 14.70551497719767475, -125.7371425972743424 ) ) ;
#1823 = DIRECTION ( 'NONE',  ( 0.000000000000000000, -0.000000000000000000, 1.000000000000000000 ) ) ;
#1824 = CARTESIAN_POINT ( 'NONE',  ( -7.653276971141075080, 13.99920316164806344, -116.4876868865759150 ) ) ;
#1825 = AXIS2_PLACEMENT_3D ( 'NONE', #13079, #2727, #2494 ) ;
#1826 = DATE_AND_TIME ( #2982, #10622 ) ;
#1827 = CIRCLE ( 'NONE', #8721, 3.000000000000011990 ) ;
#1828 = CARTESIAN_POINT ( 'NONE',  ( 13.66360635575861515, 15.00000000000000000, -125.8738101257675766 ) ) ;
#1829 =( BOUNDED_SURFACE ( )  B_SPLINE_SURFACE ( 3, 2, ( 
 ( #11691, #7042, #10380 ),
 ( #2042, #6974, #12704 ),
 ( #7984, #1108, #14096 ),
 ( #11759, #15119, #4510 ),
 ( #14020, #10601, #3417 ),
 ( #3346, #10533, #14177 ) ),
 .UNSPECIFIED., .F., .F., .T. ) 
 B_SPLINE_SURFACE_WITH_KNOTS ( ( 4, 2, 4 ),
 ( 3, 3 ),
 ( 0.000000000000000000, 0.006940540637791398938, 0.01388108127558279788 ),
 ( 0.000000000000000000, 1.000000000000000000 ),
 .UNSPECIFIED. ) 
 GEOMETRIC_REPRESENTATION_ITEM ( )  RATIONAL_B_SPLINE_SURFACE ( (
 ( 1.000000000000000000, 0.7071067811865471286, 1.000000000000000000),
 ( 1.000000000000000000, 0.7071067811865471286, 1.000000000000000000),
 ( 1.000000000000000000, 0.7071067811865475727, 1.000000000000000000),
 ( 1.000000000000000000, 0.7071067811865475727, 1.000000000000000000),
 ( 1.000000000000000000, 0.7071067811865469066, 1.000000000000000000),
 ( 1.000000000000000000, 0.7071067811865469066, 1.000000000000000000) ) ) 
 REPRESENTATION_ITEM ( '' )  SURFACE ( )  );
#1830 = ORIENTED_EDGE ( 'NONE', *, *, #6589, .F. ) ;
#1831 = CARTESIAN_POINT ( 'NONE',  ( -2.298097038856278918, 3.375000000000000000, -5.798097038856277585 ) ) ;
#1832 = CARTESIAN_POINT ( 'NONE',  ( -28.89672605278645889, 4.000000000000001776, -180.4390744492250747 ) ) ;
#1833 = CARTESIAN_POINT ( 'NONE',  ( -3.750000000000000000, 12.25000000000000000, -3.499999999999999112 ) ) ;
#1834 = ORIENTED_EDGE ( 'NONE', *, *, #320, .F. ) ;
#1835 = CARTESIAN_POINT ( 'NONE',  ( -9.203922670347713719, 11.37012112914805506, -115.4376859600374559 ) ) ;
#1836 = VECTOR ( 'NONE', #1086, 1000.000000000000000 ) ;
#1837 = AXIS2_PLACEMENT_3D ( 'NONE', #5416, #5343, #865 ) ;
#1838 = CARTESIAN_POINT ( 'NONE',  ( -3.749999999999999556, 3.187500000000000000, -1.946699141100892927 ) ) ;
#1839 = CARTESIAN_POINT ( 'NONE',  ( 7.641599596749856005, 4.009295114047140451, -21.18645330027491269 ) ) ;
#1840 = CARTESIAN_POINT ( 'NONE',  ( 0.4810967732360011406, 3.291314837355760137, 5.449392047321778065 ) ) ;
#1841 = EDGE_CURVE ( 'NONE', #6670, #6553, #10134, .T. ) ;
#1842 = CARTESIAN_POINT ( 'NONE',  ( -3.750000000000000000, 0.3125000000000000555, -5.053300858899105741 ) ) ;
#1843 = APPROVAL_STATUS ( 'not_yet_approved' ) ;
#1844 = EDGE_CURVE ( 'NONE', #12142, #2185, #3221, .T. ) ;
#1845 = CARTESIAN_POINT ( 'NONE',  ( -4.738306685235110116, 1.195290186917868924, -1.000000000000011768 ) ) ;
#1846 = CIRCLE ( 'NONE', #11944, 7.000000000000016875 ) ;
#1847 = DIRECTION ( 'NONE',  ( 0.000000000000000000, 0.000000000000000000, 1.000000000000000000 ) ) ;
#1848 = ORIENTED_EDGE ( 'NONE', *, *, #2219, .T. ) ;
#1849 = CARTESIAN_POINT ( 'NONE',  ( 5.228075279701640099, 4.000000000000000000, -165.7939279834373849 ) ) ;
#1850 = CARTESIAN_POINT ( 'NONE',  ( -3.980102097228897738E-16, 2.000000000000000000, -6.749999999999999112 ) ) ;
#1851 = CARTESIAN_POINT ( 'NONE',  ( -2.298097038856279362, 8.874999999999996447, -5.798097038856278473 ) ) ;
#1852 = CARTESIAN_POINT ( 'NONE',  ( -7.737061903549631303, 15.00000000000000888, -106.6108512366692480 ) ) ;
#1853 = APPROVAL ( #9021, 'UNSPECIFIED' ) ;
#1854 = CARTESIAN_POINT ( 'NONE',  ( 11.32911567345497872, 12.86975428404477029, -106.8195553291829185 ) ) ;
#1855 = CARTESIAN_POINT ( 'NONE',  ( 2.298097038856279362, 6.875000000000000000, -1.201902961143720860 ) ) ;
#1856 = CARTESIAN_POINT ( 'NONE',  ( -2.651650429449552870, 3.625000000000000888, -0.8483495705504467965 ) ) ;
#1857 = CARTESIAN_POINT ( 'NONE',  ( 2.651650429449553759, 8.875000000000001776, -0.8483495705504471296 ) ) ;
#1858 = CARTESIAN_POINT ( 'NONE',  ( 10.95703869986693491, 5.830414896929611679, -43.93911433197450833 ) ) ;
#1859 = CARTESIAN_POINT ( 'NONE',  ( -4.924212822021339697, 0.02956586206423728741, -117.3690025739556262 ) ) ;
#1860 = CARTESIAN_POINT ( 'NONE',  ( 2.651650429449554203, 10.37500000000000000, -0.8483495705504471296 ) ) ;
#1861 = DIRECTION ( 'NONE',  ( 1.000000000000000000, 0.000000000000000000, 0.000000000000000000 ) ) ;
#1862 = CARTESIAN_POINT ( 'NONE',  ( 30.32986759126112730, 0.7500000000000000000, 43.04214087805580391 ) ) ;
#1863 = ADVANCED_FACE ( 'NONE', ( #4320 ), #9023, .F. ) ;
#1864 = ADVANCED_FACE ( 'NONE', ( #13749 ), #1752, .T. ) ;
#1865 = CARTESIAN_POINT ( 'NONE',  ( 1.870406778884745380, 2.100000000000000089, -0.7779448751454841604 ) ) ;
#1866 = EDGE_LOOP ( 'NONE', ( #5293, #14647, #10401, #9553 ) ) ;
#1867 = CARTESIAN_POINT ( 'NONE',  ( -29.36516290028746212, -2.190758066230379322E-12, -186.4185780521328581 ) ) ;
#1868 = CARTESIAN_POINT ( 'NONE',  ( -2.298097038856278473, 0.1250000000000000000, -1.201902961143720416 ) ) ;
#1869 = CARTESIAN_POINT ( 'NONE',  ( -48.65881315193669110, 15.00000000000000000, -156.6898889965183628 ) ) ;
#1870 = CARTESIAN_POINT ( 'NONE',  ( -2.651650429449552870, 13.62500000000000000, -0.8483495705504463524 ) ) ;
#1871 = EDGE_LOOP ( 'NONE', ( #286, #1033, #7734, #5875 ) ) ;
#1872 = DIRECTION ( 'NONE',  ( -0.000000000000000000, -1.000000000000000000, -0.000000000000000000 ) ) ;
#1873 = CARTESIAN_POINT ( 'NONE',  ( 11.32016196459919755, 4.662706325538023222, -106.4092894470422408 ) ) ;
#1874 = FACE_OUTER_BOUND ( 'NONE', #12453, .T. ) ;
#1875 = CARTESIAN_POINT ( 'NONE',  ( -3.249999999999999556, 10.18750000000000000, -2.153805922287440833 ) ) ;
#1876 = LINE ( 'NONE', #7457, #4298 ) ;
#1877 = CARTESIAN_POINT ( 'NONE',  ( 2.298097038856279362, 8.375000000000000000, -1.201902961143720860 ) ) ;
#1878 = CARTESIAN_POINT ( 'NONE',  ( 20.15233411323433188, 8.673617379884035472E-16, -140.2512511322913440 ) ) ;
#1879 = CARTESIAN_POINT ( 'NONE',  ( 3.749999999999998668, 13.68750000000000000, -5.053300858899107517 ) ) ;
#1880 = CARTESIAN_POINT ( 'NONE',  ( -67.78894976056668042, 9.999999999999998224, -204.1377247873641068 ) ) ;
#1881 = CARTESIAN_POINT ( 'NONE',  ( -18.09353981420591140, -1.734723475976807094E-15, -129.3374956033358387 ) ) ;
#1882 = CARTESIAN_POINT ( 'NONE',  ( 3.249999999999998668, 13.68750000000000000, -4.846194077712560500 ) ) ;
#1883 = ADVANCED_FACE ( 'NONE', ( #4617 ), #9097, .T. ) ;
#1884 = CARTESIAN_POINT ( 'NONE',  ( -9.030574454602209755, 2.490287375297123962, -34.97919997656153157 ) ) ;
#1885 = DIRECTION ( 'NONE',  ( -0.000000000000000000, -1.000000000000000000, -0.000000000000000000 ) ) ;
#1886 = CARTESIAN_POINT ( 'NONE',  ( 3.249999999999998668, 7.687500000000000000, -4.846194077712560500 ) ) ;
#1887 = CARTESIAN_POINT ( 'NONE',  ( 3.116228908706373701, 1.920977637013419947, 4.205425761845583033 ) ) ;
#1888 = CARTESIAN_POINT ( 'NONE',  ( 10.94790802041947941, 11.56847231179307656, -43.52074019388548010 ) ) ;
#1889 = ORIENTED_EDGE ( 'NONE', *, *, #1728, .F. ) ;
#1890 = CARTESIAN_POINT ( 'NONE',  ( -0.2962205294200088712, 15.00000000000000000, -113.2751335308100096 ) ) ;
#1891 = CARTESIAN_POINT ( 'NONE',  ( -3.749999999999999556, 0.1875000000000001110, -1.946699141100892927 ) ) ;
#1892 = CARTESIAN_POINT ( 'NONE',  ( 3.249999999999998224, 15.31250000000000355, -2.153805922287439945 ) ) ;
#1893 = CARTESIAN_POINT ( 'NONE',  ( 1.346194077712561166, 14.43750000000000178, -0.2500000000000011102 ) ) ;
#1894 = ORIENTED_EDGE ( 'NONE', *, *, #4195, .T. ) ;
#1895 = CARTESIAN_POINT ( 'NONE',  ( -3.249999999999999556, 12.18750000000000000, -2.153805922287440833 ) ) ;
#1896 = CARTESIAN_POINT ( 'NONE',  ( 9.950460554352121179, 12.63099284567753777, -43.64860988872874259 ) ) ;
#1897 = CARTESIAN_POINT ( 'NONE',  ( 2.159942170319879562, 9.999999999999998224, -121.5147849362692369 ) ) ;
#1898 = CARTESIAN_POINT ( 'NONE',  ( -16.51872302133460124, 15.00000000000000000, -108.9020125831789727 ) ) ;
#1899 = CARTESIAN_POINT ( 'NONE',  ( -9.345007083234262879, 10.72273131058215867, -115.3736373665762471 ) ) ;
#1900 = PERSON_AND_ORGANIZATION ( #3176, #3020 ) ;
#1901 = CARTESIAN_POINT ( 'NONE',  ( 5.807692710371052947, 15.00000000000000000, -113.5160805275953209 ) ) ;
#1902 = CARTESIAN_POINT ( 'NONE',  ( 9.044950117654433797, 0.000000000000000000, -141.4826476090360643 ) ) ;
#1903 = CARTESIAN_POINT ( 'NONE',  ( 27.51230737804261395, 5.000000000000002665, -137.3927180530722580 ) ) ;
#1904 = EDGE_LOOP ( 'NONE', ( #3933, #12185, #4859, #13166 ) ) ;
#1905 = CARTESIAN_POINT ( 'NONE',  ( 1.346194077712560944, 4.937500000000001776, -0.2500000000000010547 ) ) ;
#1906 = CARTESIAN_POINT ( 'NONE',  ( -27.72689154219598962, 3.999999999999999112, -176.3502337898269445 ) ) ;
#1907 = CARTESIAN_POINT ( 'NONE',  ( 0.000000000000000000, 3.500000000000000000, 0.2500000000000002220 ) ) ;
#1908 = VECTOR ( 'NONE', #3112, 1000.000000000000000 ) ;
#1909 = EDGE_LOOP ( 'NONE', ( #149, #8122, #8707, #7208 ) ) ;
#1910 = CARTESIAN_POINT ( 'NONE',  ( -1.885054460532284537, 1.750000000000027311, 38.35079268139701014 ) ) ;
#1911 = CARTESIAN_POINT ( 'NONE',  ( 4.507463604512255806, 5.000000000000000000, 2.585105772303601945 ) ) ;
#1912 = CARTESIAN_POINT ( 'NONE',  ( 3.750000000000000000, 3.750000000000000000, -3.500000000000000444 ) ) ;
#1913 = CARTESIAN_POINT ( 'NONE',  ( 7.393739102816695663, 4.119861755223847233, -25.69316058899638833 ) ) ;
#1914 = CARTESIAN_POINT ( 'NONE',  ( 3.154843497088497539, 2.483716029600458786, 4.543567367663276180 ) ) ;
#1915 = CARTESIAN_POINT ( 'NONE',  ( -1.553300858899106407, 2.062500000000000000, 0.2500000000000002220 ) ) ;
#1916 = CALENDAR_DATE ( 2026, 8, 10 ) ;
#1917 = CARTESIAN_POINT ( 'NONE',  ( -4.975935430107380597, 0.2459835157955775065, -1.000000000000011990 ) ) ;
#1918 = CARTESIAN_POINT ( 'NONE',  ( -25.82983890416511841, 9.999999999999998224, -142.4527639562402328 ) ) ;
#1919 = EDGE_LOOP ( 'NONE', ( #1454, #5980, #12777, #11990, #5653, #6083, #4304, #7053, #3449, #13322, #1156, #2244 ) ) ;
#1920 = CARTESIAN_POINT ( 'NONE',  ( -68.74655823203735849, 9.999999999999998224, -201.8315121478229912 ) ) ;
#1921 = CARTESIAN_POINT ( 'NONE',  ( 2.298097038856279362, 4.375000000000000000, -1.201902961143720860 ) ) ;
#1922 = CARTESIAN_POINT ( 'NONE',  ( 7.000000000000000888, 15.00000000000000000, -1.663700395152567513 ) ) ;
#1923 = CARTESIAN_POINT ( 'NONE',  ( -6.591932536214704541, 4.336808689942017736E-16, -124.2971136505211831 ) ) ;
#1924 = ADVANCED_FACE ( 'NONE', ( #14923 ), #2216, .F. ) ;
#1925 = CARTESIAN_POINT ( 'NONE',  ( -2.651650429449552870, 5.625000000000000000, -0.8483495705504467965 ) ) ;
#1926 = CARTESIAN_POINT ( 'NONE',  ( -1.553300858899106407, 10.06250000000000000, 0.2500000000000002220 ) ) ;
#1927 = CARTESIAN_POINT ( 'NONE',  ( -6.738069272572023038, 0.6073807294375053178, -116.5044176451308999 ) ) ;
#1928 = ORIENTED_EDGE ( 'NONE', *, *, #10523, .T. ) ;
#1929 = DIRECTION ( 'NONE',  ( -0.9961255586397049777, -0.000000000000000000, 0.08794243244723004560 ) ) ;
#1930 = CARTESIAN_POINT ( 'NONE',  ( 3.749999999999999112, 11.18750000000000178, -5.053300858899108405 ) ) ;
#1931 = CARTESIAN_POINT ( 'NONE',  ( 4.284495748330572340, 14.99196994537862260, -0.3632064617744598656 ) ) ;
#1932 = CARTESIAN_POINT ( 'NONE',  ( 7.753811188820753486, -2.743867526398026335, -39.64929316069592602 ) ) ;
#1933 = FACE_OUTER_BOUND ( 'NONE', #12198, .T. ) ;
#1934 = VERTEX_POINT ( 'NONE', #3447 ) ;
#1935 = CARTESIAN_POINT ( 'NONE',  ( -20.78833667511313976, 3.151119262966928298E-15, -163.5248793559493379 ) ) ;
#1936 = CARTESIAN_POINT ( 'NONE',  ( 12.40744575253754611, 2.644372666245800918, -166.2747719090159819 ) ) ;
#1937 = CARTESIAN_POINT ( 'NONE',  ( -35.54172072644912106, 15.00000000000000000, -156.2450653136882011 ) ) ;
#1938 = CARTESIAN_POINT ( 'NONE',  ( -1.346194077712559167, 3.937500000000001332, -6.749999999999999112 ) ) ;
#1939 = ORIENTED_EDGE ( 'NONE', *, *, #2781, .F. ) ;
#1940 = CARTESIAN_POINT ( 'NONE',  ( -14.61394712176886834, 5.000000000000000888, -133.7291658263849854 ) ) ;
#1941 = DIRECTION ( 'NONE',  ( -0.000000000000000000, -1.000000000000000000, -0.000000000000000000 ) ) ;
#1942 = CARTESIAN_POINT ( 'NONE',  ( -4.781971238371357735, 9.999999999999998224, -110.8602639898391402 ) ) ;
#1943 = ADVANCED_FACE ( 'NONE', ( #11498 ), #11566, .F. ) ;
#1944 = CARTESIAN_POINT ( 'NONE',  ( 2.299001413601184485, 8.673617379884035472E-16, -109.5170782816581010 ) ) ;
#1945 = CARTESIAN_POINT ( 'NONE',  ( -3.249999999999999556, 7.750000000000000888, -3.500000000000000000 ) ) ;
#1946 = CARTESIAN_POINT ( 'NONE',  ( 21.45872126895855558, 8.673617379884035472E-16, -137.8933061875234216 ) ) ;
#1947 = CARTESIAN_POINT ( 'NONE',  ( -2.651650429449553314, 13.37500000000000000, -6.151650429449552426 ) ) ;
#1948 = CARTESIAN_POINT ( 'NONE',  ( -68.19209817244900762, 9.999999999999998224, -203.2686135453940608 ) ) ;
#1949 = CARTESIAN_POINT ( 'NONE',  ( -0.9087754948914270603, 0.000000000000000000, -36.05536862169275025 ) ) ;
#1950 = CARTESIAN_POINT ( 'NONE',  ( -3.980102097228897245E-16, 10.50000000000000000, -6.749999999999999112 ) ) ;
#1951 = DIRECTION ( 'NONE',  ( -0.8674617751425300893, 0.000000000000000000, -0.4975038378410468476 ) ) ;
#1952 = CARTESIAN_POINT ( 'NONE',  ( 3.249999999999998668, 9.687500000000000000, -4.846194077712560500 ) ) ;
#1953 = CARTESIAN_POINT ( 'NONE',  ( 2.597361546216158334, 7.589415207398532024E-16, 0.5567601655735897603 ) ) ;
#1954 = CARTESIAN_POINT ( 'NONE',  ( 3.136841903360915396, 5.000000000000000888, -104.4936450199714955 ) ) ;
#1955 = CC_DESIGN_DATE_AND_TIME_ASSIGNMENT ( #11321, #7770, ( #2439 ) ) ;
#1956 = ORIENTED_EDGE ( 'NONE', *, *, #8954, .F. ) ;
#1957 = DIRECTION ( 'NONE',  ( 0.000000000000000000, 0.000000000000000000, 1.000000000000000000 ) ) ;
#1958 = CARTESIAN_POINT ( 'NONE',  ( -20.89020113344621166, 4.000000000000000888, -201.4223823251848842 ) ) ;
#1959 = CARTESIAN_POINT ( 'NONE',  ( -1.553300858899107073, 14.93750000000000000, -7.249999999999999112 ) ) ;
#1960 = CARTESIAN_POINT ( 'NONE',  ( 1.553300858899105963, 1.062500000000000444, -7.249999999999999112 ) ) ;
#1961 = CARTESIAN_POINT ( 'NONE',  ( 2.298097038856278473, 1.625000000000000222, -5.798097038856279362 ) ) ;
#1962 = EDGE_LOOP ( 'NONE', ( #7380, #5824, #14934, #1994 ) ) ;
#1963 = EDGE_CURVE ( 'NONE', #1934, #5913, #13212, .T. ) ;
#1964 = CARTESIAN_POINT ( 'NONE',  ( -3.249999999999999556, 12.25000000000000000, -3.499999999999999556 ) ) ;
#1965 = ADVANCED_FACE ( 'NONE', ( #7938 ), #12566, .T. ) ;
#1966 = ADVANCED_FACE ( 'NONE', ( #4413 ), #10, .T. ) ;
#1967 = FACE_OUTER_BOUND ( 'NONE', #863, .T. ) ;
#1968 = CC_DESIGN_APPROVAL ( #10179, ( #4203 ) ) ;
#1969 = LINE ( 'NONE', #2192, #15083 ) ;
#1970 = PLANE ( 'NONE',  #4007 ) ;
#1971 = CARTESIAN_POINT ( 'NONE',  ( -9.079473912025640914, 11.74640706415874902, -115.4940425210668593 ) ) ;
#1972 = CIRCLE ( 'NONE', #14579, 4.000000000000002665 ) ;
#1973 = CARTESIAN_POINT ( 'NONE',  ( 6.794935331052586847, 15.00000000000000000, -119.3072837454165978 ) ) ;
#1974 = CARTESIAN_POINT ( 'NONE',  ( 2.539506111722884096, 15.00000000000000000, -24.39141914772463693 ) ) ;
#1975 = CARTESIAN_POINT ( 'NONE',  ( 24.39879083497066148, 1.007048232812085553, -137.7273893344313933 ) ) ;
#1976 = ORIENTED_EDGE ( 'NONE', *, *, #12128, .F. ) ;
#1977 = CARTESIAN_POINT ( 'NONE',  ( -3.249999999999999556, 3.250000000000000444, -3.499999999999999556 ) ) ;
#1978 = CARTESIAN_POINT ( 'NONE',  ( -30.67393154469030847, 4.000000000000000000, -191.3981176163640328 ) ) ;
#1979 = CARTESIAN_POINT ( 'NONE',  ( -3.750000000000000000, 3.687500000000000444, -1.946699141100893149 ) ) ;
#1980 = ORIENTED_EDGE ( 'NONE', *, *, #4223, .T. ) ;
#1981 = CC_DESIGN_APPROVAL ( #6787, ( #12333 ) ) ;
#1982 = CARTESIAN_POINT ( 'NONE',  ( 5.000000000000000000, 9.999999999999998224, -100.6237003951525679 ) ) ;
#1983 = DIRECTION ( 'NONE',  ( 0.000000000000000000, 1.000000000000000000, 0.000000000000000000 ) ) ;
#1984 = AXIS2_PLACEMENT_3D ( 'NONE', #9301, #8356, #6206 ) ;
#1985 = CARTESIAN_POINT ( 'NONE',  ( -4.592425496802573972E-16, 7.500000000000000000, -7.249999999999999112 ) ) ;
#1986 = CARTESIAN_POINT ( 'NONE',  ( -25.36802828785869579, 1.152219026994713014, -206.4234313139986909 ) ) ;
#1987 = CARTESIAN_POINT ( 'NONE',  ( 3.030111226435038052, 1.214660924608283343, 3.496784441768035379 ) ) ;
#1988 = CARTESIAN_POINT ( 'NONE',  ( -3.750000000000000000, 3.312500000000000000, -5.053300858899105741 ) ) ;
#1989 = APPROVAL_DATE_TIME ( #759, #2928 ) ;
#1990 = CARTESIAN_POINT ( 'NONE',  ( 8.479240049521797218, 5.000000000000000000, -112.0221658571874741 ) ) ;
#1991 = AXIS2_PLACEMENT_3D ( 'NONE', #7091, #1391, #5795 ) ;
#1992 = VECTOR ( 'NONE', #10708, 1000.000000000000000 ) ;
#1993 = CIRCLE ( 'NONE', #7913, 6.000000000000005329 ) ;
#1994 = ORIENTED_EDGE ( 'NONE', *, *, #2538, .F. ) ;
#1995 = CARTESIAN_POINT ( 'NONE',  ( 3.249999999999999556, 5.249999999999999112, -3.500000000000000000 ) ) ;
#1996 = CARTESIAN_POINT ( 'NONE',  ( -9.385448347264267355, 9.999999999999998224, -115.3551636530117150 ) ) ;
#1997 = CONICAL_SURFACE ( 'NONE', #3218, 1.000000000000000888, 0.6283185307179600665 ) ;
#1998 = CIRCLE ( 'NONE', #13078, 0.2500000000000002220 ) ;
#2000 =( BOUNDED_SURFACE ( )  B_SPLINE_SURFACE ( 3, 2, ( 
 ( #4769, #5846, #13123 ),
 ( #11947, #11794, #1293 ),
 ( #9484, #2533, #15301 ),
 ( #7234, #1372, #2838 ) ),
 .UNSPECIFIED., .F., .F., .F. ) 
 B_SPLINE_SURFACE_WITH_KNOTS ( ( 4, 4 ),
 ( 3, 3 ),
 ( 0.09990852050945690788, 0.1000240204753783668 ),
 ( 0.000000000000000000, 0.05733937959224865571 ),
 .UNSPECIFIED. ) 
 GEOMETRIC_REPRESENTATION_ITEM ( )  RATIONAL_B_SPLINE_SURFACE ( (
 ( 1.000000000000000000, 0.9832056845464598460, 0.9683373203504848092),
 ( 1.000000000000000000, 0.9832056845464598460, 0.9683373203504848092),
 ( 1.000000000000000000, 0.9832056845464598460, 0.9683373203504848092),
 ( 1.000000000000000000, 0.9832056845464598460, 0.9683373203504848092) ) ) 
 REPRESENTATION_ITEM ( '' )  SURFACE ( )  );
#1999 = CARTESIAN_POINT ( 'NONE',  ( -1.553300858899106629, 10.56250000000000355, 0.2499999999999998335 ) ) ;
#2001 = AXIS2_PLACEMENT_3D ( 'NONE', #10565, #13041, #2451 ) ;
#2002 = CARTESIAN_POINT ( 'NONE',  ( -4.592425496802573972E-16, 13.50000000000000000, -7.249999999999999112 ) ) ;
#2003 = CARTESIAN_POINT ( 'NONE',  ( -2.894992141681591136, 2.255542499959168001, -1.000000000000001332 ) ) ;
#2004 = ORIENTED_EDGE ( 'NONE', *, *, #8855, .T. ) ;
#2005 = LINE ( 'NONE', #9969, #1520 ) ;
#2006 = CARTESIAN_POINT ( 'NONE',  ( 1.346194077712558057, 8.562500000000001776, -6.750000000000000000 ) ) ;
#2007 = CARTESIAN_POINT ( 'NONE',  ( -2.651650429449553314, 9.875000000000000000, -6.151650429449552426 ) ) ;
#2008 = CARTESIAN_POINT ( 'NONE',  ( -7.400090585548307232, 4.336808689942017736E-16, -125.4022374643889464 ) ) ;
#2009 = CARTESIAN_POINT ( 'NONE',  ( -0.7011654427748897911, -2.490287375297125294, -44.24552462515097062 ) ) ;
#2010 =( BOUNDED_SURFACE ( )  B_SPLINE_SURFACE ( 3, 2, ( 
 ( #4359, #7679, #6599 ),
 ( #6672, #9067, #11238 ),
 ( #12313, #10005, #2897 ),
 ( #729, #657, #3045 ),
 ( #580, #1812, #8768 ),
 ( #1656, #5362, #500 ) ),
 .UNSPECIFIED., .F., .F., .F. ) 
 B_SPLINE_SURFACE_WITH_KNOTS ( ( 4, 2, 4 ),
 ( 3, 3 ),
 ( 0.000000000000000000, 0.001345013985307758498, 0.002690027970615516996 ),
 ( 0.000000000000000000, 1.000000000000000000 ),
 .UNSPECIFIED. ) 
 GEOMETRIC_REPRESENTATION_ITEM ( )  RATIONAL_B_SPLINE_SURFACE ( (
 ( 1.000000000000000000, 0.7071067811865477948, 1.000000000000000000),
 ( 1.000000000000000000, 0.7155213219688852933, 1.000000000000000000),
 ( 1.000000000000000000, 0.7203076836420526652, 1.000000000000000000),
 ( 1.000000000000000000, 0.7203068556383743770, 1.000000000000000000),
 ( 1.000000000000000000, 0.7155213468501946394, 1.000000000000000000),
 ( 1.000000000000000000, 0.7071067811865475727, 1.000000000000000000) ) ) 
 REPRESENTATION_ITEM ( '' )  SURFACE ( )  );
#2011 = CARTESIAN_POINT ( 'NONE',  ( 9.044950117654433797, 6.000000000000000000, -141.4826476090360643 ) ) ;
#2012 = AXIS2_PLACEMENT_3D ( 'NONE', #5865, #15179, #3481 ) ;
#2013 = EDGE_LOOP ( 'NONE', ( #7617, #7244, #3186, #12149 ) ) ;
#2014 = CARTESIAN_POINT ( 'NONE',  ( -29.80312056968273993, -8.173210768771287891E-13, -194.9698201312028232 ) ) ;
#2015 = CARTESIAN_POINT ( 'NONE',  ( 12.05350762744194171, 1.921718543347064934, -165.9463472480123016 ) ) ;
#2016 = CARTESIAN_POINT ( 'NONE',  ( -29.69515346086419427, 15.00000000000000000, -156.7390981038714699 ) ) ;
#2017 = CARTESIAN_POINT ( 'NONE',  ( 0.000000000000000000, 3.500000000000000000, -0.2500000000000002220 ) ) ;
#2018 = ORIENTED_EDGE ( 'NONE', *, *, #3173, .F. ) ;
#2019 = CARTESIAN_POINT ( 'NONE',  ( -8.749806588114527273, 10.00000000000000000, -116.1271478199639944 ) ) ;
#2020 = FACE_OUTER_BOUND ( 'NONE', #5308, .T. ) ;
#2021 = DIRECTION ( 'NONE',  ( -0.08794243244722427244, 0.000000000000000000, -0.9961255586397055328 ) ) ;
#2022 = CARTESIAN_POINT ( 'NONE',  ( 8.990769910733003911, 12.49999999999999822, 0.3250886916252367920 ) ) ;
#2023 = CARTESIAN_POINT ( 'NONE',  ( -9.476787056091271921, 5.000000000000000888, -115.4301398046334981 ) ) ;
#2024 = CARTESIAN_POINT ( 'NONE',  ( -3.980102097228897738E-16, 14.00000000000000000, -6.749999999999999112 ) ) ;
#2025 = CARTESIAN_POINT ( 'NONE',  ( 16.56640677697020436, 8.749999999999998224, -94.72203932698644735 ) ) ;
#2026 = CARTESIAN_POINT ( 'NONE',  ( -3.749999999999999556, 14.31250000000000000, -5.053300858899104853 ) ) ;
#2027 = CARTESIAN_POINT ( 'NONE',  ( -0.3766621274091715987, 0.2613176957160640579, -6.863050255469941519 ) ) ;
#2028 = CARTESIAN_POINT ( 'NONE',  ( -6.624869655310543060, 11.24276207080473888, -124.9757423372164595 ) ) ;
#2029 = CARTESIAN_POINT ( 'NONE',  ( 0.000000000000000000, 14.00000000000000000, -0.2500000000000002220 ) ) ;
#2030 = CARTESIAN_POINT ( 'NONE',  ( 22.59313949056596726, 0.2140682042508952609, -138.3733707844687331 ) ) ;
#2031 = EDGE_CURVE ( 'NONE', #2235, #688, #15022, .T. ) ;
#2032 = CARTESIAN_POINT ( 'NONE',  ( 4.439041005648131311, 14.09689541346372543, 2.512619722007936041 ) ) ;
#2033 = CARTESIAN_POINT ( 'NONE',  ( -1.346194077712559389, 9.062499999999998224, -0.2500000000000002220 ) ) ;
#2034 = CARTESIAN_POINT ( 'NONE',  ( -3.042169416580296826, 8.673617379884035472E-16, -135.1880271770022546 ) ) ;
#2035 = CARTESIAN_POINT ( 'NONE',  ( -4.492499072540820926, 5.000000000000000000, 2.611025101989610686 ) ) ;
#2036 = LOCAL_TIME ( 12, 28, 20.00000000000000000, #12824 ) ;
#2037 = ORIENTED_EDGE ( 'NONE', *, *, #13851, .F. ) ;
#2038 = ORIENTED_EDGE ( 'NONE', *, *, #9298, .T. ) ;
#2039 = CARTESIAN_POINT ( 'NONE',  ( 3.872594309009198987, 15.00000000000000000, -106.2339216993545676 ) ) ;
#2040 = CARTESIAN_POINT ( 'NONE',  ( 1.553300858899108849, 0.9374999999999998890, 0.2499999999999993616 ) ) ;
#2041 = CARTESIAN_POINT ( 'NONE',  ( 1.346194077712561166, 13.43750000000000355, -0.2500000000000011102 ) ) ;
#2042 = CARTESIAN_POINT ( 'NONE',  ( 4.047901358979359543, 9.999999999999998224, -106.4041221358673113 ) ) ;
#2043 = EDGE_LOOP ( 'NONE', ( #11614, #9520, #3342, #7597 ) ) ;
#2044 = CARTESIAN_POINT ( 'NONE',  ( 1.346194077712560944, 9.937499999999998224, -0.2500000000000010547 ) ) ;
#2045 = CARTESIAN_POINT ( 'NONE',  ( -3.305084003370867052, -2.579141538380387733, -1.000000000000001110 ) ) ;
#2046 = CARTESIAN_POINT ( 'NONE',  ( -7.344214697115496904, 13.90884050551771622, -104.3832092088654804 ) ) ;
#2047 = DIRECTION ( 'NONE',  ( 0.000000000000000000, 0.000000000000000000, -1.000000000000000000 ) ) ;
#2048 = DATE_TIME_ROLE ( 'classification_date' ) ;
#2049 = ADVANCED_FACE ( 'NONE', ( #8333 ), #9392, .T. ) ;
#2050 = CARTESIAN_POINT ( 'NONE',  ( 8.541738004602031253, 15.00000000000000178, -116.2437985782397476 ) ) ;
#2051 = CARTESIAN_POINT ( 'NONE',  ( 5.228075279701640099, 1.000000000000000000, -165.7939279834373849 ) ) ;
#2052 = VERTEX_POINT ( 'NONE', #8411 ) ;
#2053 = VECTOR ( 'NONE', #8876, 1000.000000000000114 ) ;
#2054 = EDGE_CURVE ( 'NONE', #12985, #12117, #3555, .T. ) ;
#2055 = CARTESIAN_POINT ( 'NONE',  ( 1.279752910752960382, 4.059554565823606076, -139.4003843612397020 ) ) ;
#2056 = CARTESIAN_POINT ( 'NONE',  ( -3.980102097228897245E-16, 11.50000000000000000, -6.749999999999999112 ) ) ;
#2057 = EDGE_LOOP ( 'NONE', ( #1614, #6032, #7142, #9980, #14410, #900, #13890, #5734 ) ) ;
#2058 = CARTESIAN_POINT ( 'NONE',  ( -1.346194077712559389, 3.437500000000000000, -6.749999999999999112 ) ) ;
#2059 = CARTESIAN_POINT ( 'NONE',  ( -11.98604617743635181, 4.000000000000000000, -150.3522495476669292 ) ) ;
#2060 = CARTESIAN_POINT ( 'NONE',  ( 2.651650429449554203, 2.375000000000000000, -0.8483495705504471296 ) ) ;
#2061 = ORIENTED_EDGE ( 'NONE', *, *, #2523, .F. ) ;
#2062 = DIRECTION ( 'NONE',  ( -0.9961255586397049777, -0.000000000000000000, 0.08794243244723004560 ) ) ;
#2063 = CARTESIAN_POINT ( 'NONE',  ( 4.286263797015736595E-16, 0.000000000000000000, 3.500000000000000000 ) ) ;
#2064 = CARTESIAN_POINT ( 'NONE',  ( -1.553300858899107295, 6.437500000000000888, -7.250000000000000000 ) ) ;
#2065 = AXIS2_PLACEMENT_3D ( 'NONE', #15040, #9366, #9448 ) ;
#2066 = AXIS2_PLACEMENT_3D ( 'NONE', #9354, #3562, #8192 ) ;
#2067 = B_SPLINE_CURVE_WITH_KNOTS ( 'NONE', 3,
 ( #11597, #3483, #2255, #2104 ),
 .UNSPECIFIED., .F., .F.,
 ( 4, 4 ),
 ( 0.000000000000000000, 0.0003026718941486676129 ),
 .UNSPECIFIED. ) ;
#2068 = CARTESIAN_POINT ( 'NONE',  ( -25.53589191382039658, 2.627299923236849910, -208.1764131119443846 ) ) ;
#2069 = FACE_BOUND ( 'NONE', #243, .T. ) ;
#2070 = COORDINATED_UNIVERSAL_TIME_OFFSET ( 0, 0, .AHEAD. ) ;
#2071 = CYLINDRICAL_SURFACE ( 'NONE', #4074, 0.5000000000000004441 ) ;
#2072 = ADVANCED_FACE ( 'NONE', ( #3786 ), #12860, .T. ) ;
#2073 = ORIENTED_EDGE ( 'NONE', *, *, #7235, .F. ) ;
#2074 = AXIS2_PLACEMENT_3D ( 'NONE', #4044, #4270, #8750 ) ;
#2075 = VECTOR ( 'NONE', #11847, 1000.000000000000227 ) ;
#2076 = CARTESIAN_POINT ( 'NONE',  ( -2.298097038856279362, 1.874999999999999778, -5.798097038856278473 ) ) ;
#2077 = DIRECTION ( 'NONE',  ( 0.000000000000000000, 0.000000000000000000, -1.000000000000000000 ) ) ;
#2078 = CARTESIAN_POINT ( 'NONE',  ( 2.651650429449553314, 10.37500000000000000, -0.8483495705504476847 ) ) ;
#2079 = CARTESIAN_POINT ( 'NONE',  ( 1.553300858899108849, 14.93750000000000178, 0.2499999999999993616 ) ) ;
#2080 = CARTESIAN_POINT ( 'NONE',  ( -67.21428272770161527, 14.43681881222333629, -196.2604947070364574 ) ) ;
#2081 = CARTESIAN_POINT ( 'NONE',  ( -3.862572585540200443, 9.963559498897122779, -43.53919170703361630 ) ) ;
#2082 = CARTESIAN_POINT ( 'NONE',  ( 1.553300858899105963, 14.06250000000000178, -7.250000000000000888 ) ) ;
#2083 = VECTOR ( 'NONE', #10768, 999.9999999999998863 ) ;
#2084 = CARTESIAN_POINT ( 'NONE',  ( 11.23659815053166611, 13.16053590981122312, -106.3906584630388039 ) ) ;
#2085 = CARTESIAN_POINT ( 'NONE',  ( -34.30915949386029240, -7.218191908991773431, -205.6798263580839716 ) ) ;
#2086 = CARTESIAN_POINT ( 'NONE',  ( 51.62524086895222553, 0.000000000000000000, 69.88209797381236399 ) ) ;
#2087 = ORIENTED_EDGE ( 'NONE', *, *, #5451, .T. ) ;
#2088 = CARTESIAN_POINT ( 'NONE',  ( -27.57977843586095190, -1.786917643684941595E-12, -204.3315731964443387 ) ) ;
#2089 = DIRECTION ( 'NONE',  ( 0.000000000000000000, -1.000000000000000000, 0.000000000000000000 ) ) ;
#2090 = CARTESIAN_POINT ( 'NONE',  ( -59.62538729158823969, 9.999999999999998224, -184.0486941882289784 ) ) ;
#2091 = CARTESIAN_POINT ( 'NONE',  ( -2.298097038856279362, 0.8750000000000000000, -5.798097038856278473 ) ) ;
#2092 = ORIENTED_EDGE ( 'NONE', *, *, #6406, .T. ) ;
#2093 = CARTESIAN_POINT ( 'NONE',  ( 1.169562822776721855, -2.409215066305258279, -1.000000000000001332 ) ) ;
#2094 = AXIS2_PLACEMENT_3D ( 'NONE', #9344, #15087, #13922 ) ;
#2095 =( BOUNDED_SURFACE ( )  B_SPLINE_SURFACE ( 3, 1, ( 
 ( #10450, #3116 ),
 ( #9212, #7829 ),
 ( #8121, #11534 ),
 ( #15112, #9065 ) ),
 .UNSPECIFIED., .F., .F., .F. ) 
 B_SPLINE_SURFACE_WITH_KNOTS ( ( 4, 4 ),
 ( 2, 2 ),
 ( 0.000000000000000000, 1.000000000000000000 ),
 ( 0.000000000000000000, 1.000000000000000000 ),
 .UNSPECIFIED. ) 
 GEOMETRIC_REPRESENTATION_ITEM ( )  RATIONAL_B_SPLINE_SURFACE ( (
 ( 1.000000000000000000, 1.000000000000000000),
 ( 0.9206647990551181104, 0.9206647990551181104),
 ( 0.9206647990551181104, 0.9206647990551181104),
 ( 1.000000000000000000, 1.000000000000000000) ) ) 
 REPRESENTATION_ITEM ( '' )  SURFACE ( )  );
#2096 = CARTESIAN_POINT ( 'NONE',  ( 0.2499999999999999445, 4.500000000000000888, -1.499999999999999778 ) ) ;
#2097 = AXIS2_PLACEMENT_3D ( 'NONE', #10330, #12740, #7859 ) ;
#2098 = CARTESIAN_POINT ( 'NONE',  ( 8.941075674752649860, 14.66517635709258194, 2.602113448209936841 ) ) ;
#2099 = CARTESIAN_POINT ( 'NONE',  ( 2.958795351719239797, 8.673617379884035472E-16, -108.2770199283325780 ) ) ;
#2100 = CARTESIAN_POINT ( 'NONE',  ( 1.346194077712561166, 13.43750000000000355, -0.2500000000000011102 ) ) ;
#2101 = CARTESIAN_POINT ( 'NONE',  ( -13.05415704217878670, 0.000000000000000000, -133.9853474364657870 ) ) ;
#2102 = CARTESIAN_POINT ( 'NONE',  ( 2.651650429449554203, 1.375000000000000000, -0.8483495705504471296 ) ) ;
#2103 = CIRCLE ( 'NONE', #11960, 3.500000000000000000 ) ;
#2104 = CARTESIAN_POINT ( 'NONE',  ( -0.3766621274091715432, -0.2054769798019681903, -0.1347136637304948981 ) ) ;
#2105 = CARTESIAN_POINT ( 'NONE',  ( -8.725755766768878985, 11.34072931828999309, -105.4285433685658546 ) ) ;
#2106 = CARTESIAN_POINT ( 'NONE',  ( 2.298097038856278473, 14.62500000000000000, -5.798097038856279362 ) ) ;
#2107 = CARTESIAN_POINT ( 'NONE',  ( -2.141054399116761875, 15.00000000000000000, -102.7251783244459631 ) ) ;
#2108 = CARTESIAN_POINT ( 'NONE',  ( 11.00225911879145002, 8.749999999999998224, -91.84275802117696230 ) ) ;
#2109 = CARTESIAN_POINT ( 'NONE',  ( 2.298097038856279362, 9.875000000000000000, -1.201902961143720860 ) ) ;
#2110 = CARTESIAN_POINT ( 'NONE',  ( 3.230086961373113130, 4.669421605118766472, 5.208283729180105404 ) ) ;
#2111 = CARTESIAN_POINT ( 'NONE',  ( -3.545188519422978413, 5.000000000000000000, -132.7285785787237558 ) ) ;
#2112 = VERTEX_POINT ( 'NONE', #11812 ) ;
#2113 = ORIENTED_EDGE ( 'NONE', *, *, #13782, .F. ) ;
#2114 = CARTESIAN_POINT ( 'NONE',  ( 8.554370898791335165, 8.673617379884035472E-16, -168.5027005598435039 ) ) ;
#2115 = CARTESIAN_POINT ( 'NONE',  ( -3.749999999999999556, 14.75000000000000000, -3.499999999999999112 ) ) ;
#2116 = CARTESIAN_POINT ( 'NONE',  ( 2.298097038856279362, 15.37500000000000178, -1.201902961143720860 ) ) ;
#2117 = CARTESIAN_POINT ( 'NONE',  ( 13.13192191588670887, 4.000000000000000000, -166.1703390355876877 ) ) ;
#2118 = ORIENTED_EDGE ( 'NONE', *, *, #13876, .T. ) ;
#2119 = CARTESIAN_POINT ( 'NONE',  ( -3.249999999999999556, 7.187500000000000000, -2.153805922287440833 ) ) ;
#2120 = CARTESIAN_POINT ( 'NONE',  ( -1.346194077712559167, 0.9375000000000000000, -6.749999999999999112 ) ) ;
#2121 = ADVANCED_FACE ( 'NONE', ( #10515, #14075 ), #15247, .F. ) ;
#2122 = CARTESIAN_POINT ( 'NONE',  ( -0.1117941955214328681, 5.000000000000000888, -102.1231258608400907 ) ) ;
#2123 = CARTESIAN_POINT ( 'NONE',  ( 43.47613484165132292, 2.100000000006494449, 51.22794247056654626 ) ) ;
#2124 =( NAMED_UNIT ( * ) SI_UNIT ( $, .STERADIAN. ) SOLID_ANGLE_UNIT ( ) );
#2125 = CARTESIAN_POINT ( 'NONE',  ( -1.346194077712559389, 5.062500000000001776, -0.2500000000000002220 ) ) ;
#2126 = CONTEXT_DEPENDENT_SHAPE_REPRESENTATION ( #1368, #1405 ) ;
#2127 = CARTESIAN_POINT ( 'NONE',  ( 8.459890227649916383, 12.49999999999999822, -115.7934283673321261 ) ) ;
#2128 = CARTESIAN_POINT ( 'NONE',  ( -8.506498296742877940, 13.16062949075057809, -116.6455419169648593 ) ) ;
#2129 = ORIENTED_EDGE ( 'NONE', *, *, #7120, .T. ) ;
#2130 = CARTESIAN_POINT ( 'NONE',  ( 26.20154845188031700, 2.488669359958907812, -138.3263134144609410 ) ) ;
#2131 = CARTESIAN_POINT ( 'NONE',  ( 3.249999999999999556, 10.75000000000000000, -3.500000000000000000 ) ) ;
#2132 = EDGE_LOOP ( 'NONE', ( #13908, #15093, #3361 ) ) ;
#2133 = VERTEX_POINT ( 'NONE', #5110 ) ;
#2134 = CARTESIAN_POINT ( 'NONE',  ( 2.651650429449554203, 11.37500000000000000, -0.8483495705504471296 ) ) ;
#2135 = CARTESIAN_POINT ( 'NONE',  ( 1.004809442601927394, 5.000000000000000888, -139.4752805618705622 ) ) ;
#2136 = CARTESIAN_POINT ( 'NONE',  ( -2.651650429449552870, 0.6250000000000002220, -0.8483495705504463524 ) ) ;
#2137 = CARTESIAN_POINT ( 'NONE',  ( -3.249999999999999112, 6.812500000000001776, -4.846194077712558723 ) ) ;
#2138 = EDGE_LOOP ( 'NONE', ( #1727, #4975, #10021, #10676 ) ) ;
#2139 = FACE_OUTER_BOUND ( 'NONE', #4677, .T. ) ;
#2140 = MANIFOLD_SOLID_BREP ( 'Redondeo5', #8564 ) ;
#2141 = CARTESIAN_POINT ( 'NONE',  ( 2.298097038856279362, 1.875000000000000000, -1.201902961143720860 ) ) ;
#2142 = PRODUCT_DEFINITION_SHAPE ( 'NONE', 'NONE',  #15320 ) ;
#2143 = CARTESIAN_POINT ( 'NONE',  ( 2.651650429449552870, 6.625000000000000000, -6.151650429449554203 ) ) ;
#2144 = ADVANCED_FACE ( 'NONE', ( #8502 ), #13393, .F. ) ;
#2145 = CARTESIAN_POINT ( 'NONE',  ( -25.48033468270072532, 3.216921005771350206, -208.6603374304535805 ) ) ;
#2146 = CARTESIAN_POINT ( 'NONE',  ( 10.01939027896081313, 9.999999999999998224, -127.6977514918621637 ) ) ;
#2147 = PERSON_AND_ORGANIZATION ( #3176, #3020 ) ;
#2148 = CARTESIAN_POINT ( 'NONE',  ( 21.53395630484880385, 5.000000000000001776, -133.2577068754237644 ) ) ;
#2149 = DIRECTION ( 'NONE',  ( 0.02181900108494663065, 0.000000000000000000, -0.9997619372588932851 ) ) ;
#2150 = ORIENTED_EDGE ( 'NONE', *, *, #12494, .T. ) ;
#2151 = CARTESIAN_POINT ( 'NONE',  ( 0.000000000000000000, 8.500000000000000000, -0.2500000000000002220 ) ) ;
#2152 = APPROVAL ( #5668, 'UNKNOWN' ) ;
#2153 = LINE ( 'NONE', #15073, #6492 ) ;
#2154 = EDGE_CURVE ( 'NONE', #3281, #13049, #7652, .T. ) ;
#2155 = CARTESIAN_POINT ( 'NONE',  ( -1.553300858899107073, 7.937500000000001776, -7.249999999999999112 ) ) ;
#2156 = EDGE_CURVE ( 'NONE', #1027, #7762, #11853, .T. ) ;
#2157 = CARTESIAN_POINT ( 'NONE',  ( -32.49979969806456381, 5.000000000000000000, -156.1716796081737186 ) ) ;
#2158 = EDGE_CURVE ( 'NONE', #12985, #5655, #10819, .T. ) ;
#2159 = CARTESIAN_POINT ( 'NONE',  ( -65.38695984819520390, 14.99496204924664333, -188.1638777877195707 ) ) ;
#2160 = CARTESIAN_POINT ( 'NONE',  ( -3.648797883638980277, -2.490287375297125294, -1.000000000000000888 ) ) ;
#2161 = CARTESIAN_POINT ( 'NONE',  ( 3.749999999999999556, 13.25000000000000000, -3.500000000000000444 ) ) ;
#2162 = CARTESIAN_POINT ( 'NONE',  ( -12.27209645382210823, 9.999999999999998224, -127.2227734861304782 ) ) ;
#2163 = APPROVAL_STATUS ( 'not_yet_approved' ) ;
#2164 = DIRECTION ( 'NONE',  ( -0.000000000000000000, -1.000000000000000000, -0.000000000000000000 ) ) ;
#2165 = ORIENTED_EDGE ( 'NONE', *, *, #13598, .T. ) ;
#2166 = CARTESIAN_POINT ( 'NONE',  ( -25.22286604074212235, 8.673617379884035472E-16, -198.5635032934493154 ) ) ;
#2167 = CARTESIAN_POINT ( 'NONE',  ( -1.346194077712558945, 4.062500000000000000, -0.2500000000000002220 ) ) ;
#2168 = CARTESIAN_POINT ( 'NONE',  ( -53.33476332432898914, 9.999999999999998224, -169.8150382216356320 ) ) ;
#2169 = CARTESIAN_POINT ( 'NONE',  ( -3.249999999999999112, 1.812499999999999778, -4.846194077712558723 ) ) ;
#2170 = ORIENTED_EDGE ( 'NONE', *, *, #2031, .T. ) ;
#2171 = CARTESIAN_POINT ( 'NONE',  ( 9.939878312292620421, 5.000000000000000888, -115.2320631035898373 ) ) ;
#2172 = CARTESIAN_POINT ( 'NONE',  ( 8.941148554184975339, 11.11253373586288440, 2.598774061488354103 ) ) ;
#2173 = CARTESIAN_POINT ( 'NONE',  ( -0.3214635615751804121, 1.215333660157913752E-12, -103.0394908280570405 ) ) ;
#2174 = CARTESIAN_POINT ( 'NONE',  ( -2.298097038856278029, 12.62500000000000000, -1.201902961143720638 ) ) ;
#2175 = CARTESIAN_POINT ( 'NONE',  ( 2.469015410240005259, 8.673617379884035472E-16, -109.2094522964932963 ) ) ;
#2176 = CARTESIAN_POINT ( 'NONE',  ( 1.553300858899109516, 2.437500000000000444, 0.2499999999999993616 ) ) ;
#2177 = CC_DESIGN_PERSON_AND_ORGANIZATION_ASSIGNMENT ( #9952, #9876, ( #13898 ) ) ;
#2178 = FACE_OUTER_BOUND ( 'NONE', #9307, .T. ) ;
#2179 = CARTESIAN_POINT ( 'NONE',  ( 26.66216796319303484, 4.264883946051542196, -136.8970070307220794 ) ) ;
#2180 = CARTESIAN_POINT ( 'NONE',  ( -0.7212374594705488473, 0.000000000000000000, 37.83387651873656665 ) ) ;
#2181 = CARTESIAN_POINT ( 'NONE',  ( 2.298097038856278473, 6.625000000000000000, -5.798097038856279362 ) ) ;
#2182 = CARTESIAN_POINT ( 'NONE',  ( 3.555703521826507174, 14.99969716236488182, -12.86313601129666750 ) ) ;
#2183 = FACE_OUTER_BOUND ( 'NONE', #13177, .T. ) ;
#2184 = EDGE_LOOP ( 'NONE', ( #13158, #1128, #13339, #9772 ) ) ;
#2185 = VERTEX_POINT ( 'NONE', #7418 ) ;
#2186 = CARTESIAN_POINT ( 'NONE',  ( 8.305508344667165588, 12.50000000000000000, -114.1336091688761343 ) ) ;
#2187 = CARTESIAN_POINT ( 'NONE',  ( 0.000000000000000000, 7.000000000000000000, 0.2500000000000002220 ) ) ;
#2188 = CARTESIAN_POINT ( 'NONE',  ( -1.553300858899107073, 0.9375000000000000000, -7.249999999999999112 ) ) ;
#2189 = DIRECTION ( 'NONE',  ( 0.000000000000000000, -1.000000000000000000, -0.000000000000000000 ) ) ;
#2190 = ORIENTED_EDGE ( 'NONE', *, *, #14746, .T. ) ;
#2191 = CARTESIAN_POINT ( 'NONE',  ( 3.249999999999998224, 2.312500000000000000, -2.153805922287439945 ) ) ;
#2192 = CARTESIAN_POINT ( 'NONE',  ( -67.58382170693636226, 15.00000000000000000, -204.5178482451963191 ) ) ;
#2193 = CARTESIAN_POINT ( 'NONE',  ( 1.346194077712560944, 5.937500000000000000, -0.2500000000000010547 ) ) ;
#2194 = EDGE_CURVE ( 'NONE', #9763, #4330, #4228, .T. ) ;
#2195 = DIRECTION ( 'NONE',  ( 0.000000000000000000, 0.000000000000000000, -1.000000000000000000 ) ) ;
#2196 = DIRECTION ( 'NONE',  ( -0.000000000000000000, -1.000000000000000000, -0.000000000000000000 ) ) ;
#2197 = EDGE_CURVE ( 'NONE', #6060, #2112, #9479, .T. ) ;
#2198 = ORIENTED_EDGE ( 'NONE', *, *, #8627, .F. ) ;
#2199 = CARTESIAN_POINT ( 'NONE',  ( -0.01496453197141594735, 0.000000000000000000, -5.196130874293185542 ) ) ;
#2200 = CARTESIAN_POINT ( 'NONE',  ( 2.298097038856278473, 11.62500000000000000, -5.798097038856279362 ) ) ;
#2201 = ORIENTED_EDGE ( 'NONE', *, *, #6737, .F. ) ;
#2202 = ORIENTED_EDGE ( 'NONE', *, *, #1189, .T. ) ;
#2203 = CARTESIAN_POINT ( 'NONE',  ( -1.553300858899106629, 11.56250000000000178, 0.2500000000000002220 ) ) ;
#2204 = CARTESIAN_POINT ( 'NONE',  ( -1.873266413721881518, 2.331468351712828833E-16, 1.481691765633328606 ) ) ;
#2205 = CARTESIAN_POINT ( 'NONE',  ( 0.000000000000000000, 6.500000000000000000, 0.2500000000000002220 ) ) ;
#2206 = CARTESIAN_POINT ( 'NONE',  ( -3.249999999999999112, 4.812500000000001776, -4.846194077712558723 ) ) ;
#2207 = VERTEX_POINT ( 'NONE', #3953 ) ;
#2208 = CARTESIAN_POINT ( 'NONE',  ( -0.5126277339387972365, 9.999999999999998224, -103.6859198938611399 ) ) ;
#2209 = CARTESIAN_POINT ( 'NONE',  ( -3.249999999999999556, 1.312500000000000444, -4.846194077712557835 ) ) ;
#2210 = CARTESIAN_POINT ( 'NONE',  ( 3.749999999999998668, 7.687500000000000000, -5.053300858899107517 ) ) ;
#2211 = CARTESIAN_POINT ( 'NONE',  ( -25.31370737356648348, 0.4053893758470029085, -203.6075974930378152 ) ) ;
#2212 = CARTESIAN_POINT ( 'NONE',  ( -7.160896140961710898, 10.00000000000000000, -146.2205208844301580 ) ) ;
#2213 = CALENDAR_DATE ( 2026, 8, 10 ) ;
#2214 = CARTESIAN_POINT ( 'NONE',  ( -63.21837158064308682, 15.00000000000000000, -178.6113122644988209 ) ) ;
#2215 = EDGE_CURVE ( 'NONE', #1043, #8933, #6187, .T. ) ;
#2216 = CYLINDRICAL_SURFACE ( 'NONE', #6031, 3.500000000000003109 ) ;
#2217 = CC_DESIGN_APPROVAL ( #4538, ( #11824 ) ) ;
#2218 = ORIENTED_EDGE ( 'NONE', *, *, #10940, .F. ) ;
#2219 = EDGE_CURVE ( 'NONE', #5143, #8206, #255, .T. ) ;
#2220 = CIRCLE ( 'NONE', #4688, 2.000000000000001776 ) ;
#2221 = CARTESIAN_POINT ( 'NONE',  ( -1.346194077712559167, 7.937500000000001776, -6.749999999999999112 ) ) ;
#2222 = CARTESIAN_POINT ( 'NONE',  ( 10.16835622167071840, 14.49892404887047981, -106.6099690722883082 ) ) ;
#2223 = CARTESIAN_POINT ( 'NONE',  ( -4.592425496802573972E-16, 8.000000000000000000, -7.250000000000000000 ) ) ;
#2224 = CARTESIAN_POINT ( 'NONE',  ( 3.750000000000000000, 12.75000000000000178, -3.500000000000000444 ) ) ;
#2225 = CARTESIAN_POINT ( 'NONE',  ( 3.249999999999999556, 11.75000000000000000, -3.500000000000000000 ) ) ;
#2226 = CARTESIAN_POINT ( 'NONE',  ( 3.249999999999999556, 1.750000000000000000, -3.500000000000000000 ) ) ;
#2227 = CARTESIAN_POINT ( 'NONE',  ( -65.07427810169019722, 14.43681881204452111, -196.3032221514726530 ) ) ;
#2228 = CARTESIAN_POINT ( 'NONE',  ( -4.036619102201398412, -2.193945312325716657, -1.000000000000001110 ) ) ;
#2229 = CARTESIAN_POINT ( 'NONE',  ( -3.249999999999999556, 8.250000000000000000, -3.499999999999999556 ) ) ;
#2230 = CARTESIAN_POINT ( 'NONE',  ( 0.000000000000000000, -0.4999999999999999445, -0.2500000000000002220 ) ) ;
#2231 = FACE_OUTER_BOUND ( 'NONE', #5069, .T. ) ;
#2232 = VECTOR ( 'NONE', #6285, 1000.000000000000000 ) ;
#2233 = APPROVAL_DATE_TIME ( #7154, #11527 ) ;
#2234 = DIRECTION ( 'NONE',  ( 0.000000000000000000, 0.6972771395097921987, 0.7168016397282039875 ) ) ;
#2235 = VERTEX_POINT ( 'NONE', #12293 ) ;
#2236 = EDGE_CURVE ( 'NONE', #12980, #11984, #236, .T. ) ;
#2237 = CARTESIAN_POINT ( 'NONE',  ( -28.17198374595783861, 3.576437372583847189E-12, -202.9920081940992986 ) ) ;
#2238 = CARTESIAN_POINT ( 'NONE',  ( -2.298097038856278473, 2.125000000000000000, -1.201902961143720416 ) ) ;
#2239 = EDGE_CURVE ( 'NONE', #6631, #9693, #10763, .T. ) ;
#2240 = CARTESIAN_POINT ( 'NONE',  ( -63.02554947701982968, 9.999999999999998224, -201.1265914030773843 ) ) ;
#2241 = EDGE_CURVE ( 'NONE', #6383, #12545, #3461, .T. ) ;
#2242 = AXIS2_PLACEMENT_3D ( 'NONE', #2744, #4063, #12164 ) ;
#2243 = CARTESIAN_POINT ( 'NONE',  ( 3.249999999999998224, 3.312500000000000000, -2.153805922287439945 ) ) ;
#2244 = ORIENTED_EDGE ( 'NONE', *, *, #6102, .T. ) ;
#2245 = CARTESIAN_POINT ( 'NONE',  ( 1.114947364559086829, 15.00000000000000000, -139.4079432275550232 ) ) ;
#2246 = CIRCLE ( 'NONE', #13847, 5.000000000000000000 ) ;
#2247 = CARTESIAN_POINT ( 'NONE',  ( -25.50370618284765456, 2.956430103652706531, -208.4658715182746391 ) ) ;
#2248 = CARTESIAN_POINT ( 'NONE',  ( -4.037064903932549242, 8.673617379884035472E-16, -173.3783848444354021 ) ) ;
#2249 = APPROVAL ( #12305, 'UNSPECIFIED' ) ;
#2250 = CARTESIAN_POINT ( 'NONE',  ( 0.000000000000000000, 5.000000000000000888, -100.6237003951525537 ) ) ;
#2251 = CARTESIAN_POINT ( 'NONE',  ( 2.298097038856279362, 13.37500000000000000, -1.201902961143720860 ) ) ;
#2252 = CARTESIAN_POINT ( 'NONE',  ( 10.58692965144313014, 0.000000000000000000, -159.5308220099450409 ) ) ;
#2253 = CARTESIAN_POINT ( 'NONE',  ( 1.553300858899105963, 1.062500000000000444, -7.250000000000000888 ) ) ;
#2254 = PERSON ( 'NAUO-PER6', 'UNSPECIFIED', 'UNSPECIFIED', ('UNSPECIFIED'), ('UNSPECIFIED'), ('UNSPECIFIED') ) ;
#2255 = CARTESIAN_POINT ( 'NONE',  ( -0.3766621274094114624, -0.2521619801956713203, -0.04364880428836830084 ) ) ;
#2256 = AXIS2_PLACEMENT_3D ( 'NONE', #9939, #1597, #4079 ) ;
#2257 = DIRECTION ( 'NONE',  ( 0.000000000000000000, 1.000000000000000000, 0.000000000000000000 ) ) ;
#2258 = CARTESIAN_POINT ( 'NONE',  ( 23.25775510017668424, 0.4289495323832013263, -138.1373351626023975 ) ) ;
#2259 = CARTESIAN_POINT ( 'NONE',  ( 25.24449781760964129, 2.100000000000000089, 70.71481607157352300 ) ) ;
#2260 = CARTESIAN_POINT ( 'NONE',  ( -1.346194077712559389, 14.43750000000000000, -6.749999999999999112 ) ) ;
#2261 = ADVANCED_FACE ( 'NONE', ( #2944 ), #9667, .F. ) ;
#2262 = CARTESIAN_POINT ( 'NONE',  ( 0.3766621274091715987, -0.2500000000000000000, -6.863050255469941519 ) ) ;
#2263 = FACE_OUTER_BOUND ( 'NONE', #5972, .T. ) ;
#2264 = EDGE_LOOP ( 'NONE', ( #2985, #423, #13054, #6040 ) ) ;
#2265 = ORIENTED_EDGE ( 'NONE', *, *, #11673, .F. ) ;
#2266 = CARTESIAN_POINT ( 'NONE',  ( -9.846744731551831720, 4.000000000000000888, -186.2620189933751647 ) ) ;
#2267 = CARTESIAN_POINT ( 'NONE',  ( 3.749999999999998668, 3.687500000000000444, -5.053300858899107517 ) ) ;
#2268 = CARTESIAN_POINT ( 'NONE',  ( 3.749999999999998668, 5.187499999999999112, -5.053300858899108405 ) ) ;
#2269 = DIRECTION ( 'NONE',  ( 0.000000000000000000, 1.000000000000000000, 0.000000000000000000 ) ) ;
#2270 = ORIENTED_EDGE ( 'NONE', *, *, #2909, .F. ) ;
#2271 = AXIS2_PLACEMENT_3D ( 'NONE', #8010, #10629, #8234 ) ;
#2272 = CARTESIAN_POINT ( 'NONE',  ( 3.249999999999998224, 1.187499999999999778, -4.846194077712561388 ) ) ;
#2273 = CARTESIAN_POINT ( 'NONE',  ( -49.70557948942859383, 14.99999999999999467, -143.6055563704040026 ) ) ;
#2274 = CARTESIAN_POINT ( 'NONE',  ( 38.25296960060443752, 0.000000000000000000, 42.65758570601111188 ) ) ;
#2275 =( LENGTH_UNIT ( ) NAMED_UNIT ( * ) SI_UNIT ( .MILLI., .METRE. ) );
#2276 = CARTESIAN_POINT ( 'NONE',  ( -3.249999999999999556, 5.250000000000000000, -3.499999999999999556 ) ) ;
#2277 = CALENDAR_DATE ( 2026, 8, 10 ) ;
#2278 = CARTESIAN_POINT ( 'NONE',  ( 9.335939850627564596, 15.00000000000000000, -105.2901324735335891 ) ) ;
#2279 = CARTESIAN_POINT ( 'NONE',  ( 13.25562203902501146, 5.000000000000000888, -125.4200107876433918 ) ) ;
#2280 = ORIENTED_EDGE ( 'NONE', *, *, #5172, .F. ) ;
#2281 = CARTESIAN_POINT ( 'NONE',  ( -1.509598306946452917, 15.00000000000000000, -120.1442827665486135 ) ) ;
#2282 = CARTESIAN_POINT ( 'NONE',  ( 3.249999999999999556, 9.750000000000000000, -3.500000000000000000 ) ) ;
#2283 = ORIENTED_EDGE ( 'NONE', *, *, #9491, .F. ) ;
#2284 = ORIENTED_EDGE ( 'NONE', *, *, #10998, .F. ) ;
#2285 = CARTESIAN_POINT ( 'NONE',  ( 3.749999999999999556, 10.25000000000000178, -3.500000000000000444 ) ) ;
#2286 = CARTESIAN_POINT ( 'NONE',  ( -29.74068399868164647, 4.000000000000000888, -200.7425342145079412 ) ) ;
#2287 = CARTESIAN_POINT ( 'NONE',  ( -2.651650429449553314, 3.875000000000000444, -6.151650429449552426 ) ) ;
#2288 = CARTESIAN_POINT ( 'NONE',  ( 0.000000000000000000, 6.500000000000000000, -0.2500000000000002220 ) ) ;
#2289 = VERTEX_POINT ( 'NONE', #6186 ) ;
#2290 = B_SPLINE_CURVE_WITH_KNOTS ( 'NONE', 3,
 ( #1474, #6190, #2640, #7344 ),
 .UNSPECIFIED., .F., .F.,
 ( 4, 4 ),
 ( 0.000000000000000000, 0.0003021952495015066973 ),
 .UNSPECIFIED. ) ;
#2291 = CARTESIAN_POINT ( 'NONE',  ( 0.7716514365830442479, 14.99999999999999822, -111.8714012163870564 ) ) ;
#2292 = CARTESIAN_POINT ( 'NONE',  ( 3.249999999999999112, 3.812500000000000000, -2.153805922287439945 ) ) ;
#2293 = CARTESIAN_POINT ( 'NONE',  ( -2.651650429449552870, 8.125000000000000000, -0.8483495705504462414 ) ) ;
#2294 = CARTESIAN_POINT ( 'NONE',  ( -25.46814831223248277, 0.6176455659345582161, -204.7850756988478338 ) ) ;
#2295 = CARTESIAN_POINT ( 'NONE',  ( 2.399330854043891126, -6.071532165918825619E-15, -131.2813267747279440 ) ) ;
#2296 = VECTOR ( 'NONE', #2879, 999.9999999999998863 ) ;
#2297 = CARTESIAN_POINT ( 'NONE',  ( -5.813579972774820526, -2.743867526398026335, -44.04909082593601966 ) ) ;
#2298 = PERSON_AND_ORGANIZATION_ROLE ( 'creator' ) ;
#2299 = DIRECTION ( 'NONE',  ( 0.9961255586397054218, -0.000000000000000000, -0.08794243244722428632 ) ) ;
#2300 = ORIENTED_EDGE ( 'NONE', *, *, #5832, .F. ) ;
#2301 = CARTESIAN_POINT ( 'NONE',  ( 0.000000000000000000, 5.500000000000000000, -0.2500000000000002220 ) ) ;
#2302 = FACE_OUTER_BOUND ( 'NONE', #12938, .T. ) ;
#2303 = AXIS2_PLACEMENT_3D ( 'NONE', #1982, #9169, #10322 ) ;
#2304 = EDGE_CURVE ( 'NONE', #7276, #5674, #7459, .T. ) ;
#2305 = CARTESIAN_POINT ( 'NONE',  ( -1.553300858899106629, 7.562500000000000888, 0.2499999999999998335 ) ) ;
#2306 = CARTESIAN_POINT ( 'NONE',  ( -1.553300858899107073, 14.43750000000000000, -7.250000000000000000 ) ) ;
#2307 = EDGE_CURVE ( 'NONE', #14034, #6631, #2734, .T. ) ;
#2308 = CARTESIAN_POINT ( 'NONE',  ( -66.14601255874971741, 14.98129325284761215, -196.3414374098033193 ) ) ;
#2309 = CARTESIAN_POINT ( 'NONE',  ( -0.5658740575277120266, 1.810181481809467696, -138.1533701416837800 ) ) ;
#2310 = CARTESIAN_POINT ( 'NONE',  ( 1.346194077712558279, 0.06250000000000016653, -6.750000000000000888 ) ) ;
#2311 = MANIFOLD_SOLID_BREP ( 'Redondeo1', #11529 ) ;
#2312 = CARTESIAN_POINT ( 'NONE',  ( -1.500000000000000000, 5.000000000000000000, 0.2500000000000002220 ) ) ;
#2313 = CALENDAR_DATE ( 2026, 8, 10 ) ;
#2314 = VECTOR ( 'NONE', #2596, 1000.000000000000000 ) ;
#2315 = DIRECTION ( 'NONE',  ( 0.9997619372588932851, -0.000000000000000000, 0.02181900108494707474 ) ) ;
#2316 = CIRCLE ( 'NONE', #2824, 3.000000000000005329 ) ;
#2317 = EDGE_LOOP ( 'NONE', ( #11165, #10698, #4534, #2746 ) ) ;
#2318 = CARTESIAN_POINT ( 'NONE',  ( 8.915781819284724463, 4.487270727378674273, 2.843881670126054306 ) ) ;
#2319 = CARTESIAN_POINT ( 'NONE',  ( 1.346194077712560944, 2.937500000000000000, -0.2500000000000011102 ) ) ;
#2320 =( BOUNDED_SURFACE ( )  B_SPLINE_SURFACE ( 3, 1, ( 
 ( #11721, #9482 ),
 ( #7470, #448 ),
 ( #11101, #522 ),
 ( #603, #375 ) ),
 .UNSPECIFIED., .F., .F., .F. ) 
 B_SPLINE_SURFACE_WITH_KNOTS ( ( 4, 4 ),
 ( 2, 2 ),
 ( 0.000000000000000000, 1.000000000000000000 ),
 ( 0.000000000000000000, 1.000000000000000000 ),
 .UNSPECIFIED. ) 
 GEOMETRIC_REPRESENTATION_ITEM ( )  RATIONAL_B_SPLINE_SURFACE ( (
 ( 1.000000000000000000, 1.000000000000000000),
 ( 0.9216682375510407699, 0.9216682375510407699),
 ( 0.9216682375510407699, 0.9216682375510407699),
 ( 1.000000000000000000, 1.000000000000000000) ) ) 
 REPRESENTATION_ITEM ( '' )  SURFACE ( )  );
#2321 = CARTESIAN_POINT ( 'NONE',  ( -55.02646020061353482, 15.00000000000000000, -163.3737094562771972 ) ) ;
#2322 = CARTESIAN_POINT ( 'NONE',  ( 0.000000000000000000, 8.500000000000000000, -0.2500000000000002220 ) ) ;
#2323 = ORIENTED_EDGE ( 'NONE', *, *, #4424, .T. ) ;
#2324 = CARTESIAN_POINT ( 'NONE',  ( -1.406912714274181297, 15.00000000000000000, -119.8620791452180185 ) ) ;
#2325 = CARTESIAN_POINT ( 'NONE',  ( -25.16238623267244989, 0.0006965968045201811161, -199.2040625880622997 ) ) ;
#2326 = CARTESIAN_POINT ( 'NONE',  ( 8.915609759151768898, 13.95926557866610018, 3.768979567163230460 ) ) ;
#2327 = CARTESIAN_POINT ( 'NONE',  ( 0.000000000000000000, 1.000000000000000000, -0.2500000000000002220 ) ) ;
#2328 = AXIS2_PLACEMENT_3D ( 'NONE', #11887, #151, #222 ) ;
#2329 = CARTESIAN_POINT ( 'NONE',  ( -2.298097038856279362, 11.87500000000000000, -5.798097038856278473 ) ) ;
#2330 = EDGE_CURVE ( 'NONE', #3581, #4145, #11123, .T. ) ;
#2331 = CARTESIAN_POINT ( 'NONE',  ( 3.558820106718695975, 8.673617379884034486E-16, -107.0002797207564100 ) ) ;
#2332 = CARTESIAN_POINT ( 'NONE',  ( -3.749999999999999556, 2.750000000000000444, -3.499999999999999112 ) ) ;
#2333 = DIRECTION ( 'NONE',  ( -0.000000000000000000, -1.000000000000000000, -0.000000000000000000 ) ) ;
#2334 = CARTESIAN_POINT ( 'NONE',  ( 9.939878312292615092, 5.000000000000000888, -115.2320631035898373 ) ) ;
#2335 = DIRECTION ( 'NONE',  ( -0.08794243244722420305, -1.868163743359636407E-15, -0.9961255586397055328 ) ) ;
#2336 = CARTESIAN_POINT ( 'NONE',  ( 3.390724094347318029, 11.60484605096695532, 4.922330974931754533 ) ) ;
#2337 = CARTESIAN_POINT ( 'NONE',  ( 2.298097038856278473, 12.62500000000000000, -5.798097038856279362 ) ) ;
#2338 = AXIS2_PLACEMENT_3D ( 'NONE', #3259, #12540, #6438 ) ;
#2339 = CARTESIAN_POINT ( 'NONE',  ( 1.855481649321460091, 15.00000000000000000, -35.83830032691798095 ) ) ;
#2340 = CARTESIAN_POINT ( 'NONE',  ( 6.049910241306251990, 8.673617379884035472E-16, -118.3734240199295300 ) ) ;
#2341 = ORIENTED_EDGE ( 'NONE', *, *, #14255, .F. ) ;
#2342 = ORIENTED_EDGE ( 'NONE', *, *, #12922, .T. ) ;
#2343 = DIRECTION ( 'NONE',  ( 0.02181900108494707127, 0.000000000000000000, -0.9997619372588931741 ) ) ;
#2344 = CARTESIAN_POINT ( 'NONE',  ( 2.651650429449552870, 5.625000000000000000, -6.151650429449554203 ) ) ;
#2345 = CARTESIAN_POINT ( 'NONE',  ( -2.651650429449552870, 3.625000000000000888, -0.8483495705504467965 ) ) ;
#2346 = CARTESIAN_POINT ( 'NONE',  ( 0.000000000000000000, 0.000000000000000000, 0.000000000000000000 ) ) ;
#2347 = ORIENTED_EDGE ( 'NONE', *, *, #6925, .F. ) ;
#2348 = CARTESIAN_POINT ( 'NONE',  ( -3.249999999999999112, 1.812499999999999778, -4.846194077712558723 ) ) ;
#2349 = FACE_BOUND ( 'NONE', #12167, .T. ) ;
#2350 = ADVANCED_FACE ( 'NONE', ( #12520 ), #2484, .T. ) ;
#2351 = CARTESIAN_POINT ( 'NONE',  ( 7.439269063064413601, 8.673617379884033500E-16, -125.9756671148725360 ) ) ;
#2352 = CARTESIAN_POINT ( 'NONE',  ( -2.298097038856278918, 3.375000000000000000, -5.798097038856277585 ) ) ;
#2353 = DATE_AND_TIME ( #8214, #4697 ) ;
#2354 = FACE_OUTER_BOUND ( 'NONE', #9758, .T. ) ;
#2355 = CARTESIAN_POINT ( 'NONE',  ( 8.895820146784114257, 5.000000000000000888, -117.6809082909101960 ) ) ;
#2356 = ORIENTED_EDGE ( 'NONE', *, *, #10729, .F. ) ;
#2357 = CARTESIAN_POINT ( 'NONE',  ( -17.32624372123753886, 0.000000000000000000, -122.3796757791585321 ) ) ;
#2358 = CARTESIAN_POINT ( 'NONE',  ( 6.436143463598922310, 15.00000000000000000, 2.800833825385760090 ) ) ;
#2359 = EDGE_LOOP ( 'NONE', ( #2645, #13183, #3473, #5234, #9733, #15217, #4209, #1188, #4900 ) ) ;
#2360 = ORIENTED_EDGE ( 'NONE', *, *, #13576, .T. ) ;
#2361 = CARTESIAN_POINT ( 'NONE',  ( -0.7212374594705489583, 2.331468351712828340E-16, 37.83387651873656665 ) ) ;
#2362 = CARTESIAN_POINT ( 'NONE',  ( -3.750000000000000000, 7.812500000000000000, -5.053300858899105741 ) ) ;
#2363 = CARTESIAN_POINT ( 'NONE',  ( 1.346194077712561166, 8.437500000000000000, -0.2500000000000011102 ) ) ;
#2364 = EDGE_LOOP ( 'NONE', ( #11780, #14151, #12930, #13139 ) ) ;
#2365 = CARTESIAN_POINT ( 'NONE',  ( -2.027137927901855097, 9.999999999999998224, -107.0032022124461122 ) ) ;
#2366 = CARTESIAN_POINT ( 'NONE',  ( -2.298097038856278473, 3.125000000000000000, -1.201902961143720416 ) ) ;
#2367 = CARTESIAN_POINT ( 'NONE',  ( 2.651650429449552870, 10.62500000000000000, -6.151650429449554203 ) ) ;
#2368 = CARTESIAN_POINT ( 'NONE',  ( -8.933522129290233593, 9.999999999999998224, -119.2934400955039251 ) ) ;
#2369 = CARTESIAN_POINT ( 'NONE',  ( 6.025425613339945308, 10.00000000000000355, -132.6130656762864248 ) ) ;
#2370 = FACE_BOUND ( 'NONE', #4813, .T. ) ;
#2371 = APPROVAL_ROLE ( '' ) ;
#2372 = CARTESIAN_POINT ( 'NONE',  ( -46.71028124165312079, 15.00000000000000000, -147.6754287972959503 ) ) ;
#2373 = ORIENTED_EDGE ( 'NONE', *, *, #4618, .F. ) ;
#2374 = LINE ( 'NONE', #8165, #2794 ) ;
#2375 = CARTESIAN_POINT ( 'NONE',  ( -1.553300858899107073, 12.93750000000000178, -7.249999999999999112 ) ) ;
#2376 = FACE_OUTER_BOUND ( 'NONE', #531, .T. ) ;
#2377 = CARTESIAN_POINT ( 'NONE',  ( -65.21504661764039668, 14.99629524799717650, -187.1630048673123383 ) ) ;
#2378 = CYLINDRICAL_SURFACE ( 'NONE', #782, 3.000000000000005329 ) ;
#2379 = CARTESIAN_POINT ( 'NONE',  ( -2.298097038856278029, 0.6250000000000002220, -1.201902961143720638 ) ) ;
#2380 = CARTESIAN_POINT ( 'NONE',  ( 9.246414981748314332, 0.9484790359934494042, -106.0253644157543249 ) ) ;
#2381 = PERSON_AND_ORGANIZATION ( #3176, #3020 ) ;
#2382 = PRODUCT_DEFINITION_SHAPE ( 'NONE', 'NONE',  #15317 ) ;
#2383 = CARTESIAN_POINT ( 'NONE',  ( 2.863878713867060277, 15.00000000000000000, -24.41542356333742703 ) ) ;
#2384 = DIRECTION ( 'NONE',  ( 1.000000000000000000, 0.000000000000000000, 0.000000000000000000 ) ) ;
#2385 = ORIENTED_EDGE ( 'NONE', *, *, #8923, .T. ) ;
#2386 = CARTESIAN_POINT ( 'NONE',  ( -26.89045353704901942, -1.363139722109709093E-13, -205.6554657723100945 ) ) ;
#2387 = CARTESIAN_POINT ( 'NONE',  ( -2.298097038856278918, 2.375000000000000000, -5.798097038856277585 ) ) ;
#2388 = CARTESIAN_POINT ( 'NONE',  ( -53.69697306016067273, 14.99999999999731948, -170.4167521506885237 ) ) ;
#2389 = CARTESIAN_POINT ( 'NONE',  ( 0.000000000000000000, 6.500000000000000000, -0.2500000000000002220 ) ) ;
#2390 = ORIENTED_EDGE ( 'NONE', *, *, #13032, .T. ) ;
#2391 = CARTESIAN_POINT ( 'NONE',  ( -7.119867912801005616, 9.999999999999998224, -107.3464651432735195 ) ) ;
#2392 = CLOSED_SHELL ( 'NONE', ( #6961, #2606, #9238, #9817, #10544, #4049, #1772, #14023, #6015, #5597, #643, #8244, #13312, #3294, #6173, #4241, #1366, #5743, #3178, #8056 ) ) ;
#2393 = CARTESIAN_POINT ( 'NONE',  ( -0.3766621274091715987, 0.5000000000000000000, -7.146945437571387671 ) ) ;
#2394 = CARTESIAN_POINT ( 'NONE',  ( 9.442321227527154193, 14.94013921602285855, -106.0014341817649495 ) ) ;
#2395 = CARTESIAN_POINT ( 'NONE',  ( -3.249999999999999556, 1.250000000000000000, -3.499999999999999556 ) ) ;
#2396 = CARTESIAN_POINT ( 'NONE',  ( 3.749999999999998668, 1.187499999999999778, -5.053300858899108405 ) ) ;
#2397 = CARTESIAN_POINT ( 'NONE',  ( 2.651650429449552870, 3.625000000000000000, -6.151650429449554203 ) ) ;
#2398 = CARTESIAN_POINT ( 'NONE',  ( -0.2500000000000000555, 4.500000000000000888, -0.2499999999999997780 ) ) ;
#2399 = CARTESIAN_POINT ( 'NONE',  ( -1.553300858899107073, 0.9375000000000002220, -7.249999999999999112 ) ) ;
#2400 = CARTESIAN_POINT ( 'NONE',  ( -16.94138229547581531, 5.000000000000000000, -154.2864167784019571 ) ) ;
#2401 = DIRECTION ( 'NONE',  ( -0.2611699024796619306, 0.000000000000000000, -0.9652928478129131351 ) ) ;
#2402 = CYLINDRICAL_SURFACE ( 'NONE', #11085, 5.000000000000000000 ) ;
#2403 = CARTESIAN_POINT ( 'NONE',  ( -4.488583703910701495, 2.100000000000000089, 2.894752896148880428 ) ) ;
#2404 = CARTESIAN_POINT ( 'NONE',  ( 0.000000000000000000, 12.00000000000000000, -0.2500000000000002220 ) ) ;
#2405 = CARTESIAN_POINT ( 'NONE',  ( 47.72094894359807427, 1.749999999998650191, 60.44734918181273997 ) ) ;
#2406 = CARTESIAN_POINT ( 'NONE',  ( -65.03433155014064937, 14.91485314970007003, -188.6938424094274751 ) ) ;
#2407 = ORIENTED_EDGE ( 'NONE', *, *, #2737, .F. ) ;
#2408 = EDGE_CURVE ( 'NONE', #15312, #411, #14086, .T. ) ;
#2409 = ORIENTED_EDGE ( 'NONE', *, *, #5347, .T. ) ;
#2410 = CARTESIAN_POINT ( 'NONE',  ( -2.902626628659604968, 4.336808689942017736E-16, -110.5536484212200463 ) ) ;
#2411 = CARTESIAN_POINT ( 'NONE',  ( 8.305142154013848810, 12.50000000000000000, -113.6818879023987137 ) ) ;
#2412 = CARTESIAN_POINT ( 'NONE',  ( 3.749999999999998668, 5.687500000000000000, -5.053300858899107517 ) ) ;
#2413 = CARTESIAN_POINT ( 'NONE',  ( 1.553300858899105963, 4.062500000000001776, -7.249999999999999112 ) ) ;
#2414 = CARTESIAN_POINT ( 'NONE',  ( -16.94138229547582242, 9.999999999999998224, -154.2864167784019003 ) ) ;
#2415 = ORIENTED_EDGE ( 'NONE', *, *, #3077, .F. ) ;
#2416 = CARTESIAN_POINT ( 'NONE',  ( 3.249999999999999556, 14.75000000000000178, -3.500000000000000000 ) ) ;
#2417 = CARTESIAN_POINT ( 'NONE',  ( -7.128555860240339825, 5.000000000000001776, -113.3867792963409471 ) ) ;
#2418 = CARTESIAN_POINT ( 'NONE',  ( 1.004809442601927394, 6.000000000000000000, -139.4752805618705622 ) ) ;
#2419 =( NAMED_UNIT ( * ) SI_UNIT ( $, .STERADIAN. ) SOLID_ANGLE_UNIT ( ) );
#2420 = CARTESIAN_POINT ( 'NONE',  ( 3.249999999999999112, 5.812500000000000000, -2.153805922287439945 ) ) ;
#2421 = CONTEXT_DEPENDENT_SHAPE_REPRESENTATION ( #10062, #1279 ) ;
#2422 = CC_DESIGN_DATE_AND_TIME_ASSIGNMENT ( #4299, #670, ( #7881 ) ) ;
#2423 = DIRECTION ( 'NONE',  ( 0.000000000000000000, -1.000000000000000000, 0.000000000000000000 ) ) ;
#2424 = CARTESIAN_POINT ( 'NONE',  ( -44.21823081166466096, 15.00000000000000000, -145.3603131190973272 ) ) ;
#2425 = ORIENTED_EDGE ( 'NONE', *, *, #11774, .T. ) ;
#2426 = FACE_OUTER_BOUND ( 'NONE', #14314, .T. ) ;
#2427 = DIRECTION ( 'NONE',  ( -0.3090169943749621062, 0.000000000000000000, -0.9510565162951489793 ) ) ;
#2428 = ORIENTED_EDGE ( 'NONE', *, *, #12357, .F. ) ;
#2429 = ADVANCED_FACE ( 'NONE', ( #6647 ), #5937, .T. ) ;
#2430 = ORIENTED_EDGE ( 'NONE', *, *, #10165, .T. ) ;
#2431 = CARTESIAN_POINT ( 'NONE',  ( -27.89696216417192787, 4.000000000000000888, -205.5469850651400918 ) ) ;
#2432 = CARTESIAN_POINT ( 'NONE',  ( 2.651650429449552870, 4.125000000000000000, -6.151650429449555091 ) ) ;
#2433 = EDGE_CURVE ( 'NONE', #12487, #12545, #11214, .T. ) ;
#2434 = CARTESIAN_POINT ( 'NONE',  ( -2.298097038856279362, 4.875000000000000000, -5.798097038856278473 ) ) ;
#2436 = ADVANCED_FACE ( 'NONE', ( #5562 ), #10494, .T. ) ;
#2435 = ORIENTED_EDGE ( 'NONE', *, *, #14894, .T. ) ;
#2437 = DIRECTION ( 'NONE',  ( 0.000000000000000000, 0.000000000000000000, -1.000000000000000000 ) ) ;
#2438 = CARTESIAN_POINT ( 'NONE',  ( 3.249999999999998668, 4.687500000000000888, -4.846194077712560500 ) ) ;
#2439 = PRODUCT_DEFINITION ( 'UNKNOWN', '', #10116, #12530 ) ;
#2440 = CARTESIAN_POINT ( 'NONE',  ( -6.224392388573470214, 2.500000000000000000, -108.7152457258569314 ) ) ;
#2441 = CARTESIAN_POINT ( 'NONE',  ( 10.89963103874143791, 0.4779808835687370805, -164.5338399313753257 ) ) ;
#2442 = VECTOR ( 'NONE', #5189, 1000.000000000000000 ) ;
#2443 = CARTESIAN_POINT ( 'NONE',  ( 10.22352057816269699, 15.00000000000000000, -125.5112093480189657 ) ) ;
#2444 = DATE_AND_TIME ( #13036, #7391 ) ;
#2445 = B_SPLINE_CURVE_WITH_KNOTS ( 'NONE', 3,
 ( #7854, #681, #2851, #11034, #1839, #11103, #5387, #14838, #4162, #4237, #7551, #14687, #14764, #6320, #13670, #608, #3069, #5239, #7783, #5160, #8864, #12496, #1913, #5466, #14918, #12269 ),
 .UNSPECIFIED., .F., .F.,
 ( 4, 2, 2, 2, 2, 2, 2, 2, 2, 2, 2, 2, 4 ),
 ( 0.000000000000000000, 0.0009121890263906905130, 0.001368283539586035444, 0.001824378052781380592, 0.002280472565976725523, 0.002736567079172070888, 0.003648756105562761184, 0.004560945131953451914, 0.005017039645148801616, 0.005473134158344152185, 0.005929228671539501887, 0.006385323184734852456, 0.007297512211125546655 ),
 .UNSPECIFIED. ) ;
#2446 = CARTESIAN_POINT ( 'NONE',  ( 0.3766621274091715987, 0.5000000000000000000, -6.863050255469941519 ) ) ;
#2447 = EDGE_LOOP ( 'NONE', ( #15060, #8323, #15035, #4487, #11630, #11580, #12081, #7847, #824, #765 ) ) ;
#2448 = APPLICATION_CONTEXT ( 'configuration controlled 3d designs of mechanical parts and assemblies' ) ;
#2449 = CARTESIAN_POINT ( 'NONE',  ( 8.673617379884035472E-16, 15.00000000000000000, -1.663700395152567513 ) ) ;
#2450 = CARTESIAN_POINT ( 'NONE',  ( -1.553300858899106629, 13.56250000000000000, 0.2499999999999998335 ) ) ;
#2451 = DIRECTION ( 'NONE',  ( 0.000000000000000000, 0.000000000000000000, 1.000000000000000000 ) ) ;
#2452 = CARTESIAN_POINT ( 'NONE',  ( -63.36957375107780877, 11.34385781002516858, -203.2580046453681177 ) ) ;
#2453 = CARTESIAN_POINT ( 'NONE',  ( -9.242581453897864563, 4.999999999999996447, -118.3503833458025127 ) ) ;
#2454 = CARTESIAN_POINT ( 'NONE',  ( 3.249999999999998224, 4.312500000000000000, -2.153805922287439945 ) ) ;
#2455 = CARTESIAN_POINT ( 'NONE',  ( 7.799741786693411782, 0.2423173772441938045, -105.6274327777687745 ) ) ;
#2456 = COORDINATED_UNIVERSAL_TIME_OFFSET ( 0, 0, .AHEAD. ) ;
#2457 = CC_DESIGN_APPROVAL ( #10017, ( #8872 ) ) ;
#2458 = CARTESIAN_POINT ( 'NONE',  ( 1.346194077712558057, 14.56250000000000000, -6.750000000000000000 ) ) ;
#2459 = CARTESIAN_POINT ( 'NONE',  ( -16.85248002973657577, 0.2716729216455838203, -130.7235999261775419 ) ) ;
#2460 = AXIS2_PLACEMENT_3D ( 'NONE', #4582, #9289, #3411 ) ;
#2461 = ORIENTED_EDGE ( 'NONE', *, *, #7434, .F. ) ;
#2462 = CARTESIAN_POINT ( 'NONE',  ( 4.354212728048433512, 0.4612449236405465336, 1.472775563304803415 ) ) ;
#2463 = CARTESIAN_POINT ( 'NONE',  ( -3.249999999999999556, 1.187500000000000000, -2.153805922287440833 ) ) ;
#2464 = CARTESIAN_POINT ( 'NONE',  ( -9.172836789864245333, 1.744788764959713134, -105.1340277003996846 ) ) ;
#2465 = CARTESIAN_POINT ( 'NONE',  ( -1.346194077712559167, 4.937500000000000888, -6.749999999999999112 ) ) ;
#2466 = ORIENTED_EDGE ( 'NONE', *, *, #7191, .F. ) ;
#2467 = B_SPLINE_CURVE_WITH_KNOTS ( 'NONE', 3,
 ( #5927, #8322, #10652, #13214, #2459, #67, #9493, #10799 ),
 .UNSPECIFIED., .F., .F.,
 ( 4, 2, 2, 4 ),
 ( 3.497257266061400950E-18, 0.001156836261567012903, 0.001735254392350513934, 0.002313672523134014964 ),
 .UNSPECIFIED. ) ;
#2468 = CARTESIAN_POINT ( 'NONE',  ( -5.365035937071200856, 15.00000000000000000, -111.0566899280935473 ) ) ;
#2469 = CARTESIAN_POINT ( 'NONE',  ( 0.000000000000000000, 0.000000000000000000, 0.000000000000000000 ) ) ;
#2470 = ORGANIZATION ( 'NAUO-ORG2', 'UNSPECIFIED', 'UNSPECIFIED' ) ;
#2471 = CARTESIAN_POINT ( 'NONE',  ( 6.020998550614976352, 9.999999999999998224, -132.6181299100964281 ) ) ;
#2472 = CARTESIAN_POINT ( 'NONE',  ( -3.249999999999999556, 1.187500000000000444, -2.153805922287440833 ) ) ;
#2473 = CARTESIAN_POINT ( 'NONE',  ( -3.750000000000000000, 2.687500000000000888, -1.946699141100893149 ) ) ;
#2474 = AXIS2_PLACEMENT_3D ( 'NONE', #13489, #5052, #338 ) ;
#2475 = CARTESIAN_POINT ( 'NONE',  ( 3.750000000000000000, 6.750000000000000000, -3.500000000000000444 ) ) ;
#2476 = CARTESIAN_POINT ( 'NONE',  ( 17.33677725112149304, 2.336213234116637878E-12, -156.7678757840980097 ) ) ;
#2477 = CARTESIAN_POINT ( 'NONE',  ( -2.651650429449552870, 6.625000000000000888, -0.8483495705504463524 ) ) ;
#2478 = CARTESIAN_POINT ( 'NONE',  ( 3.821717871283383250, 14.91756675554889888, 1.043977372916836233 ) ) ;
#2479 = CARTESIAN_POINT ( 'NONE',  ( 0.000000000000000000, 0.000000000000000000, 0.000000000000000000 ) ) ;
#2480 = DIRECTION ( 'NONE',  ( 0.000000000000000000, 0.000000000000000000, 1.000000000000000000 ) ) ;
#2481 = AXIS2_PLACEMENT_3D ( 'NONE', #13179, #12468, #14810 ) ;
#2482 = CARTESIAN_POINT ( 'NONE',  ( -5.137055953098589534, 8.673617379884034486E-16, -145.0199091983525648 ) ) ;
#2483 = CARTESIAN_POINT ( 'NONE',  ( 3.249999999999999556, 13.75000000000000000, -3.500000000000000000 ) ) ;
#2484 = TOROIDAL_SURFACE ( 'NONE', #11617, 11.99999999999994138, 5.000000000000000000 ) ;
#2485 = CARTESIAN_POINT ( 'NONE',  ( 13.13192191588670887, 4.000000000000000000, -166.1703390355876877 ) ) ;
#2486 = CARTESIAN_POINT ( 'NONE',  ( -64.96257786778912191, 14.30082101381936788, -197.2009545595533382 ) ) ;
#2487 = CIRCLE ( 'NONE', #3465, 3.500000000000000000 ) ;
#2488 = ORIENTED_EDGE ( 'NONE', *, *, #8197, .F. ) ;
#2489 = ORIENTED_EDGE ( 'NONE', *, *, #1558, .F. ) ;
#2490 = CARTESIAN_POINT ( 'NONE',  ( -6.947321920531724260, 4.336808689942017736E-16, -120.0269581757037969 ) ) ;
#2491 = CARTESIAN_POINT ( 'NONE',  ( -0.7011654427748897911, -2.490287375297126626, -44.24552462515097062 ) ) ;
#2492 = CARTESIAN_POINT ( 'NONE',  ( 3.749999999999999112, 6.812500000000000000, -1.946699141100892039 ) ) ;
#2493 = CARTESIAN_POINT ( 'NONE',  ( 1.553300858899109071, 2.437500000000000444, 0.2499999999999989175 ) ) ;
#2494 = DIRECTION ( 'NONE',  ( -1.000000000000000000, 1.224646799147353454E-16, 0.000000000000000000 ) ) ;
#2495 = ORIENTED_EDGE ( 'NONE', *, *, #4220, .F. ) ;
#2496 = CARTESIAN_POINT ( 'NONE',  ( -6.385995564645482681, 0.4374612817417152244, -116.6487767744768291 ) ) ;
#2497 = CARTESIAN_POINT ( 'NONE',  ( -1.346194077712558945, 3.562500000000000888, -0.2500000000000002220 ) ) ;
#2498 = AXIS2_PLACEMENT_3D ( 'NONE', #13285, #3852, #7312 ) ;
#2499 =( BOUNDED_SURFACE ( )  B_SPLINE_SURFACE ( 3, 2, ( 
 ( #11526, #942, #1164 ),
 ( #5645, #4723, #10363 ),
 ( #12213, #13232, #3636 ),
 ( #13387, #10814, #8498 ),
 ( #11895, #1396, #9748 ),
 ( #2634, #86, #10669 ),
 ( #6099, #13307, #5030 ),
 ( #2792, #13149, #10980 ),
 ( #3792, #8416, #6180 ),
 ( #8574, #230, #159 ),
 ( #7336, #12134, #14307 ),
 ( #12047, #2559, #7261 ),
 ( #1550, #397, #10899 ),
 ( #11976, #4797, #14553 ),
 ( #14476, #2709, #8653 ),
 ( #7495, #4946, #9510 ),
 ( #14393, #5945, #1319 ),
 ( #7412, #6023, #1467 ),
 ( #9661, #315, #3873 ),
 ( #14234, #6264, #8338 ),
 ( #13063, #2478, #7174 ),
 ( #3949, #10744, #4868 ),
 ( #9580, #5106, #3708 ),
 ( #9821, #1931, #10048 ),
 ( #7869, #5334, #14632 ),
 ( #547, #12289, #14784 ),
 ( #5485, #629, #14710 ),
 ( #4110, #8811, #11208 ) ),
 .UNSPECIFIED., .F., .F., .F. ) 
 B_SPLINE_SURFACE_WITH_KNOTS ( ( 4, 2, 2, 2, 2, 2, 2, 2, 2, 2, 2, 2, 2, 4 ),
 ( 3, 3 ),
 ( 0.000000000000000000, 0.0003810285474897536721, 0.0007620570949795073441, 0.001143085642469261016, 0.001333599916214137961, 0.001524114189959014688, 0.001905142737448768360, 0.002286171284938522032, 0.003048228379918029377, 0.003429256927407782832, 0.003810285474897536721, 0.004572342569877044065, 0.005334399664856551843, 0.006096456759836058753 ),
 ( 0.000000000000000000, 1.000000000000000000 ),
 .UNSPECIFIED. ) 
 GEOMETRIC_REPRESENTATION_ITEM ( )  RATIONAL_B_SPLINE_SURFACE ( (
 ( 1.000000000000000000, 0.6693962893781428836, 1.000000000000000000),
 ( 1.000000000000000000, 0.6693969518177473876, 1.000000000000000000),
 ( 1.000000000000000000, 0.6717808526532893509, 1.000000000000000000),
 ( 1.000000000000000000, 0.6807237459914237121, 1.000000000000000000),
 ( 1.000000000000000000, 0.6873971151302553650, 1.000000000000000000),
 ( 1.000000000000000000, 0.7036635658348195932, 1.000000000000000000),
 ( 1.000000000000000000, 0.7132100160774622610, 1.000000000000000000),
 ( 1.000000000000000000, 0.7289110705425655423, 1.000000000000000000),
 ( 1.000000000000000000, 0.7344009482827760227, 1.000000000000000000),
 ( 1.000000000000000000, 0.7455531118719149752, 1.000000000000000000),
 ( 1.000000000000000000, 0.7512296405307345992, 1.000000000000000000),
 ( 1.000000000000000000, 0.7684203367994919542, 1.000000000000000000),
 ( 1.000000000000000000, 0.7800900503501072558, 1.000000000000000000),
 ( 1.000000000000000000, 0.8032919924401181744, 1.000000000000000000),
 ( 1.000000000000000000, 0.8148697721608513245, 1.000000000000000000),
 ( 1.000000000000000000, 0.8479710425742933433, 1.000000000000000000),
 ( 1.000000000000000000, 0.8681360573711495165, 1.000000000000000000),
 ( 1.000000000000000000, 0.8947228763049550615, 1.000000000000000000),
 ( 1.000000000000000000, 0.9030109035537770001, 1.000000000000000000),
 ( 1.000000000000000000, 0.9180946610702154231, 1.000000000000000000),
 ( 1.000000000000000000, 0.9249162233022707458, 1.000000000000000000),
 ( 1.000000000000000000, 0.9433494181431361092, 1.000000000000000000),
 ( 1.000000000000000000, 0.9529202612203482303, 1.000000000000000000),
 ( 1.000000000000000000, 0.9675496472389664149, 1.000000000000000000),
 ( 1.000000000000000000, 0.9726176721090025179, 1.000000000000000000),
 ( 1.000000000000000000, 0.9792068586059596846, 1.000000000000000000),
 ( 1.000000000000000000, 0.9807988706699215520, 1.000000000000000000),
 ( 1.000000000000000000, 0.9810773865977512331, 1.000000000000000000) ) ) 
 REPRESENTATION_ITEM ( '' )  SURFACE ( )  );
#2500 = CARTESIAN_POINT ( 'NONE',  ( -63.69159315069311589, 15.00000000000000711, -164.7787203862777119 ) ) ;
#2501 = CARTESIAN_POINT ( 'NONE',  ( 10.57895993728494410, 8.673617379884033500E-16, -129.9860179236332840 ) ) ;
#2502 = EDGE_CURVE ( 'NONE', #6131, #13895, #14758, .T. ) ;
#2503 = CARTESIAN_POINT ( 'NONE',  ( 1.346194077712558057, 6.562500000000000000, -6.750000000000000000 ) ) ;
#2504 = CARTESIAN_POINT ( 'NONE',  ( -17.32624372123753886, 15.00000000000000000, -134.3796757791585037 ) ) ;
#2505 = COORDINATED_UNIVERSAL_TIME_OFFSET ( 0, 0, .AHEAD. ) ;
#2506 = CARTESIAN_POINT ( 'NONE',  ( 51.19063959271458231, 0.000000000000000000, 70.62932606827693860 ) ) ;
#2507 = CARTESIAN_POINT ( 'NONE',  ( 20.93263444590049005, 5.000000000000000888, -132.7914611339006683 ) ) ;
#2508 = EDGE_LOOP ( 'NONE', ( #10659, #8618, #8000, #4039, #6161, #4005 ) ) ;
#2509 = CARTESIAN_POINT ( 'NONE',  ( -0.8180164960865539125, 15.00000000000000355, -108.7420331879183806 ) ) ;
#2510 = DIRECTION ( 'NONE',  ( -0.9510565162951475360, 0.000000000000000000, 0.3090169943749664916 ) ) ;
#2511 =( GEOMETRIC_REPRESENTATION_CONTEXT ( 3 ) GLOBAL_UNCERTAINTY_ASSIGNED_CONTEXT ( ( #1226 ) ) GLOBAL_UNIT_ASSIGNED_CONTEXT ( ( #10465, #10390, #14104 ) ) REPRESENTATION_CONTEXT ( 'NONE', 'WORKASPACE' ) );
#2512 = ORIENTED_EDGE ( 'NONE', *, *, #11115, .T. ) ;
#2513 = EDGE_LOOP ( 'NONE', ( #6314, #3750 ) ) ;
#2514 = LINE ( 'NONE', #15213, #844 ) ;
#2515 = CARTESIAN_POINT ( 'NONE',  ( -3.750000000000000000, 5.812500000000000888, -5.053300858899105741 ) ) ;
#2516 = APPROVAL ( #13525, 'UNSPECIFIED' ) ;
#2517 = CARTESIAN_POINT ( 'NONE',  ( 2.298097038856279362, 9.374999999999998224, -1.201902961143720860 ) ) ;
#2518 = VERTEX_POINT ( 'NONE', #4827 ) ;
#2519 = CARTESIAN_POINT ( 'NONE',  ( 6.445944033997953682, 15.00000000000000355, 0.5979964941558831848 ) ) ;
#2520 = CARTESIAN_POINT ( 'NONE',  ( -1.346194077712559389, 8.437500000000000000, -6.749999999999999112 ) ) ;
#2521 = CC_DESIGN_APPROVAL ( #4519, ( #10417 ) ) ;
#2522 = LINE ( 'NONE', #6063, #11110 ) ;
#2523 = EDGE_CURVE ( 'NONE', #9024, #7289, #4899, .T. ) ;
#2524 = CARTESIAN_POINT ( 'NONE',  ( -48.29558554489104694, 10.00000000000000000, -163.1462384615805661 ) ) ;
#2525 = EDGE_CURVE ( 'NONE', #12117, #1578, #7925, .T. ) ;
#2526 = SHAPE_DEFINITION_REPRESENTATION ( #15114, #12380 ) ;
#2527 = CARTESIAN_POINT ( 'NONE',  ( 30.96695154071790412, 8.773889247172311556, -44.17511166891541308 ) ) ;
#2528 = ORIENTED_EDGE ( 'NONE', *, *, #2502, .F. ) ;
#2529 = LOCAL_TIME ( 12, 28, 20.00000000000000000, #11106 ) ;
#2530 = DIRECTION ( 'NONE',  ( -0.000000000000000000, -1.000000000000000000, -0.000000000000000000 ) ) ;
#2531 = CARTESIAN_POINT ( 'NONE',  ( 2.651650429449553314, 13.37500000000000000, -0.8483495705504476847 ) ) ;
#2532 = AXIS2_PLACEMENT_3D ( 'NONE', #560, #9981, #14720 ) ;
#2533 = CARTESIAN_POINT ( 'NONE',  ( 1.041036260628390275, 4.793811891163896277, -139.4530670678220474 ) ) ;
#2534 = CARTESIAN_POINT ( 'NONE',  ( -63.21788648181868098, 10.23658426860817450, -203.5961373993322070 ) ) ;
#2535 = CARTESIAN_POINT ( 'NONE',  ( -3.486117781607304345, 5.000000000000000000, -110.4977313129625145 ) ) ;
#2536 = CARTESIAN_POINT ( 'NONE',  ( -1.346194077712559167, 1.937500000000000222, -6.749999999999999112 ) ) ;
#2537 = CARTESIAN_POINT ( 'NONE',  ( 8.370726826406757581, 0.4830037559535477754, -105.8718434674591578 ) ) ;
#2538 = EDGE_CURVE ( 'NONE', #14191, #13258, #11772, .T. ) ;
#2539 = PERSON_AND_ORGANIZATION ( #3176, #3020 ) ;
#2540 = CARTESIAN_POINT ( 'NONE',  ( 1.346194077712560944, 14.93750000000000178, -0.2500000000000010547 ) ) ;
#2541 = DIRECTION ( 'NONE',  ( -0.000000000000000000, 0.000000000000000000, 1.000000000000000000 ) ) ;
#2542 = ORIENTED_EDGE ( 'NONE', *, *, #9382, .F. ) ;
#2543 = CARTESIAN_POINT ( 'NONE',  ( 6.189785629711340498, 0.5131405437846897621, 0.8071071970720852251 ) ) ;
#2544 = CARTESIAN_POINT ( 'NONE',  ( -1.346194077712558945, 6.062500000000000000, -0.2500000000000002220 ) ) ;
#2545 = CIRCLE ( 'NONE', #3282, 3.500000000000003109 ) ;
#2546 = CARTESIAN_POINT ( 'NONE',  ( -69.52160476852847637, 9.999999999999998224, -184.5417721423968658 ) ) ;
#2547 = CARTESIAN_POINT ( 'NONE',  ( -2.298097038856279362, 0.8750000000000000000, -5.798097038856278473 ) ) ;
#2548 = CARTESIAN_POINT ( 'NONE',  ( 3.249999999999999556, 6.250000000000000888, -3.500000000000000000 ) ) ;
#2549 = EDGE_LOOP ( 'NONE', ( #8450, #13961, #14833, #1818 ) ) ;
#2550 = CARTESIAN_POINT ( 'NONE',  ( -5.893421222750781396, 15.00000000000000000, -117.5694263798266235 ) ) ;
#2551 = CARTESIAN_POINT ( 'NONE',  ( 3.602241438175835864, 14.80771583330521501, -0.3334354230429009136 ) ) ;
#2552 = CARTESIAN_POINT ( 'NONE',  ( 2.222606327615985311, 15.00000000000000000, -129.3650357597884977 ) ) ;
#2553 = CARTESIAN_POINT ( 'NONE',  ( 1.346194077712558057, 2.562500000000000444, -6.750000000000000000 ) ) ;
#2554 = CARTESIAN_POINT ( 'NONE',  ( -2.651650429449552870, 1.874999999999999778, -6.151650429449552426 ) ) ;
#2555 = CARTESIAN_POINT ( 'NONE',  ( -1.553300858899107073, 7.437500000000000888, -7.250000000000000000 ) ) ;
#2556 = CARTESIAN_POINT ( 'NONE',  ( -4.098362961180376907, 10.53209361196889660, -46.33236032746155075 ) ) ;
#2557 = CARTESIAN_POINT ( 'NONE',  ( 2.651650429449554203, 5.375000000000000888, -0.8483495705504471296 ) ) ;
#2558 = AXIS2_PLACEMENT_3D ( 'NONE', #6039, #4884, #9595 ) ;
#2559 = CARTESIAN_POINT ( 'NONE',  ( 1.983632224063564431, 13.89821908686047180, 3.968066076948724596 ) ) ;
#2560 = CIRCLE ( 'NONE', #12671, 9.800000000000252953 ) ;
#2561 = DIRECTION ( 'NONE',  ( 0.000000000000000000, 0.000000000000000000, 1.000000000000000000 ) ) ;
#2562 = FACE_OUTER_BOUND ( 'NONE', #12563, .T. ) ;
#2563 = CARTESIAN_POINT ( 'NONE',  ( -4.512114784912129473, 6.000000000000000000, -130.1824886095253646 ) ) ;
#2564 = CARTESIAN_POINT ( 'NONE',  ( -2.298097038856278918, 12.37500000000000000, -5.798097038856277585 ) ) ;
#2565 = CARTESIAN_POINT ( 'NONE',  ( 3.717577911061880958, 0.000000000000000000, -143.6771719914432879 ) ) ;
#2566 = CARTESIAN_POINT ( 'NONE',  ( -64.07033394082162658, 14.99612073371410226, -182.3557358624200333 ) ) ;
#2567 = ORIENTED_EDGE ( 'NONE', *, *, #10264, .F. ) ;
#2568 = CARTESIAN_POINT ( 'NONE',  ( -3.750000000000000000, 9.687500000000000000, -1.946699141100893149 ) ) ;
#2569 = ORIENTED_EDGE ( 'NONE', *, *, #1020, .F. ) ;
#2570 = CARTESIAN_POINT ( 'NONE',  ( -5.948205887597929120, 4.336808689942017736E-16, -109.2829347068713588 ) ) ;
#2571 = CARTESIAN_POINT ( 'NONE',  ( 9.458437899194636955, -1.020558061026470176, -40.77697206847473410 ) ) ;
#2572 = CARTESIAN_POINT ( 'NONE',  ( 2.651650429449553759, 8.875000000000001776, -0.8483495705504471296 ) ) ;
#2573 = VECTOR ( 'NONE', #15019, 1000.000000000000000 ) ;
#2574 = CARTESIAN_POINT ( 'NONE',  ( 3.749999999999998668, 3.187500000000000444, -5.053300858899108405 ) ) ;
#2575 = AXIS2_PLACEMENT_3D ( 'NONE', #9445, #1105, #7107 ) ;
#2576 = CARTESIAN_POINT ( 'NONE',  ( 5.133649534803208070, 1.750000000002257083, 6.659653797658318553 ) ) ;
#2577 = ORIENTED_EDGE ( 'NONE', *, *, #5243, .T. ) ;
#2578 = CARTESIAN_POINT ( 'NONE',  ( -3.249999999999999112, 2.812500000000000444, -4.846194077712558723 ) ) ;
#2579 = CARTESIAN_POINT ( 'NONE',  ( -70.08092325099204345, 15.00000000000000000, -193.7014402726163098 ) ) ;
#2580 = CARTESIAN_POINT ( 'NONE',  ( 4.634195662811253946, 8.673617379884033500E-16, -120.6336223843100868 ) ) ;
#2581 = CARTESIAN_POINT ( 'NONE',  ( 1.346194077712560944, 6.937500000000000000, -0.2500000000000010547 ) ) ;
#2582 = VECTOR ( 'NONE', #2680, 1000.000000000000000 ) ;
#2583 = CARTESIAN_POINT ( 'NONE',  ( 1.320501113854922082, 4.999999999999995559, -137.8664870916820178 ) ) ;
#2584 = FACE_OUTER_BOUND ( 'NONE', #478, .T. ) ;
#2585 = VERTEX_POINT ( 'NONE', #14428 ) ;
#2586 = CARTESIAN_POINT ( 'NONE',  ( -0.4453226528549816265, -2.225540348348185052E-17, 2.000000000000000000 ) ) ;
#2587 = CARTESIAN_POINT ( 'NONE',  ( 30.32986759126112730, 1.750000000000000000, 41.04214087805579680 ) ) ;
#2588 = ORIENTED_EDGE ( 'NONE', *, *, #9905, .F. ) ;
#2589 = VERTEX_POINT ( 'NONE', #10772 ) ;
#2590 = CARTESIAN_POINT ( 'NONE',  ( 0.000000000000000000, 5.000000000000000000, 0.000000000000000000 ) ) ;
#2591 = CARTESIAN_POINT ( 'NONE',  ( 3.749999999999999112, 14.31250000000000355, -1.946699141100893149 ) ) ;
#2592 = CARTESIAN_POINT ( 'NONE',  ( 3.249999999999999556, 8.250000000000000000, -3.500000000000000000 ) ) ;
#2593 = CARTESIAN_POINT ( 'NONE',  ( 3.249999999999998224, 10.18750000000000533, -4.846194077712561388 ) ) ;
#2594 = VERTEX_POINT ( 'NONE', #9539 ) ;
#2595 = EDGE_CURVE ( 'NONE', #5598, #3495, #9611, .T. ) ;
#2596 = DIRECTION ( 'NONE',  ( 0.000000000000000000, 1.000000000000000000, -0.000000000000000000 ) ) ;
#2597 =( BOUNDED_CURVE ( )  B_SPLINE_CURVE ( 3, ( #5527, #13802, #1974, #13960 ),
 .UNSPECIFIED., .F., .F. ) 
 B_SPLINE_CURVE_WITH_KNOTS ( ( 4, 4 ),
 ( 1.375929886000936797, 1.570796326794898112 ),
 .UNSPECIFIED. ) 
 CURVE ( )  GEOMETRIC_REPRESENTATION_ITEM ( )  RATIONAL_B_SPLINE_CURVE ( ( 1.000000000000000000, 0.9968380917696022525, 0.9968380917696022525, 1.000000000000000000 ) ) 
 REPRESENTATION_ITEM ( '' )  );
#2598 = CARTESIAN_POINT ( 'NONE',  ( 2.298097038856279362, 6.875000000000000000, -1.201902961143720860 ) ) ;
#2599 = CARTESIAN_POINT ( 'NONE',  ( -9.552951302357074681, 2.499999999999999556, -124.0972072810879041 ) ) ;
#2600 = CARTESIAN_POINT ( 'NONE',  ( -61.91367734689292490, 10.00000000000000355, -193.6436493912471803 ) ) ;
#2601 = CARTESIAN_POINT ( 'NONE',  ( -66.44604053271804389, 10.00000000000000000, -157.9117883361228394 ) ) ;
#2602 = COORDINATED_UNIVERSAL_TIME_OFFSET ( 0, 0, .AHEAD. ) ;
#2603 = CARTESIAN_POINT ( 'NONE',  ( -25.21953614097411034, 0.8110625423123717370, -205.0088040713835369 ) ) ;
#2604 = ORIENTED_EDGE ( 'NONE', *, *, #12449, .T. ) ;
#2605 = CARTESIAN_POINT ( 'NONE',  ( 3.249999999999998224, 13.31250000000000178, -2.153805922287439945 ) ) ;
#2606 = ADVANCED_FACE ( 'NONE', ( #13260 ), #13096, .T. ) ;
#2607 = CARTESIAN_POINT ( 'NONE',  ( -11.27598888897756346, 0.000000000000000000, -40.77697206847459910 ) ) ;
#2608 = ADVANCED_FACE ( 'NONE', ( #12951 ), #1427, .T. ) ;
#2609 = CARTESIAN_POINT ( 'NONE',  ( 3.749999999999998668, 15.18750000000000355, -5.053300858899108405 ) ) ;
#2610 = CARTESIAN_POINT ( 'NONE',  ( -64.14881251011775021, 13.49284722309304030, -210.1482316909753365 ) ) ;
#2611 = CARTESIAN_POINT ( 'NONE',  ( 13.78275167297412906, 13.34157715675068623, -126.2206732457524794 ) ) ;
#2612 = CARTESIAN_POINT ( 'NONE',  ( 2.298097038856279362, 2.375000000000000000, -1.201902961143720860 ) ) ;
#2613 = CARTESIAN_POINT ( 'NONE',  ( 11.04510349467952146, 3.336188342164840392, -106.3259430280883322 ) ) ;
#2614 = DATE_AND_TIME ( #13368, #2529 ) ;
#2615 = CARTESIAN_POINT ( 'NONE',  ( -26.78870578381917866, 15.00000000000000000, -139.1599602021251769 ) ) ;
#2616 = LINE ( 'NONE', #7318, #13359 ) ;
#2617 = ORIENTED_EDGE ( 'NONE', *, *, #6065, .F. ) ;
#2618 = CARTESIAN_POINT ( 'NONE',  ( 8.555302993508680842, 3.062150894005132962, 2.628411868347194869 ) ) ;
#2619 = CARTESIAN_POINT ( 'NONE',  ( 2.298097038856279362, 8.875000000000001776, -1.201902961143720860 ) ) ;
#2620 = CARTESIAN_POINT ( 'NONE',  ( -8.243994158936985173, 15.00000000000000000, -104.7509493499769917 ) ) ;
#2621 = CARTESIAN_POINT ( 'NONE',  ( -1.346194077712559389, 13.06250000000000000, -0.2500000000000002220 ) ) ;
#2622 = EDGE_CURVE ( 'NONE', #7022, #7777, #3594, .T. ) ;
#2623 = CARTESIAN_POINT ( 'NONE',  ( 1.346194077712561166, 8.437500000000000000, -0.2500000000000011102 ) ) ;
#2624 = CARTESIAN_POINT ( 'NONE',  ( -5.365035937023899137, 9.999999999999998224, -111.0566899280839834 ) ) ;
#2625 = EDGE_CURVE ( 'NONE', #6350, #9880, #14611, .T. ) ;
#2626 = CARTESIAN_POINT ( 'NONE',  ( 26.71007981443199952, 6.000000000000000000, -136.8791680534710054 ) ) ;
#2627 = EDGE_CURVE ( 'NONE', #3762, #11999, #7419, .T. ) ;
#2628 = CARTESIAN_POINT ( 'NONE',  ( 8.990769910733003911, 15.00000000000000000, 0.3250886916252364589 ) ) ;
#2629 = DIRECTION ( 'NONE',  ( 0.000000000000000000, -1.000000000000000000, 0.000000000000000000 ) ) ;
#2630 = CARTESIAN_POINT ( 'NONE',  ( 1.553300858899105963, 3.062500000000000000, -7.249999999999999112 ) ) ;
#2631 = CARTESIAN_POINT ( 'NONE',  ( 0.000000000000000000, 5.000000000000000000, 0.2500000000000002220 ) ) ;
#2632 = CARTESIAN_POINT ( 'NONE',  ( -4.222954148114340889, 9.650666666666662508, -47.83347973032346090 ) ) ;
#2633 = CARTESIAN_POINT ( 'NONE',  ( -1.553300858899106629, 7.562500000000000888, 0.2500000000000002220 ) ) ;
#2634 = CARTESIAN_POINT ( 'NONE',  ( 3.422362696586258579, 11.71486000144306416, 4.863683519685648271 ) ) ;
#2635 = CARTESIAN_POINT ( 'NONE',  ( 11.39998925557648413, 0.9113012638559210288, -165.1104261359550662 ) ) ;
#2636 = CARTESIAN_POINT ( 'NONE',  ( -7.260202548253541721, 0.06312176567927152426, -104.4756693458776482 ) ) ;
#2637 = CARTESIAN_POINT ( 'NONE',  ( -5.917161057971962457, 8.673617379884035472E-16, -151.2264619204686937 ) ) ;
#2638 = DIRECTION ( 'NONE',  ( -0.04581719776170027625, 0.000000000000000000, 0.9989498407774363153 ) ) ;
#2639 = CARTESIAN_POINT ( 'NONE',  ( -23.03755312564397073, 8.673617379884035472E-16, -178.0552937557089592 ) ) ;
#2640 = CARTESIAN_POINT ( 'NONE',  ( 0.3766621274094206773, 0.2481712481078264254, -6.953504530381456661 ) ) ;
#2641 = AXIS2_PLACEMENT_3D ( 'NONE', #5355, #13492, #5210 ) ;
#2642 = ORIENTED_EDGE ( 'NONE', *, *, #14826, .F. ) ;
#2643 = PRODUCT_DEFINITION_SHAPE ( 'NONE', 'NONE',  #9258 ) ;
#2644 = CARTESIAN_POINT ( 'NONE',  ( 3.749999999999999556, 11.25000000000000000, -3.500000000000000444 ) ) ;
#2645 = ORIENTED_EDGE ( 'NONE', *, *, #7438, .T. ) ;
#2646 = CARTESIAN_POINT ( 'NONE',  ( -5.462587733769669107, 2.500000000000000444, -110.6302725851820128 ) ) ;
#2647 = CARTESIAN_POINT ( 'NONE',  ( 5.376486659670670853, 0.000000000000000000, -45.55632290616389923 ) ) ;
#2648 = CARTESIAN_POINT ( 'NONE',  ( -3.749999999999999556, 7.312500000000000888, -5.053300858899104853 ) ) ;
#2649 = CARTESIAN_POINT ( 'NONE',  ( 3.749999999999999556, 6.250000000000000000, -3.500000000000000444 ) ) ;
#2650 = CARTESIAN_POINT ( 'NONE',  ( -18.09353981420494151, 2.500000000000000444, -129.3374956033359240 ) ) ;
#2651 = VERTEX_POINT ( 'NONE', #13641 ) ;
#2652 = CARTESIAN_POINT ( 'NONE',  ( -7.369174163213311424, 0.8229795343181387501, -116.5771123024643714 ) ) ;
#2653 = CARTESIAN_POINT ( 'NONE',  ( -3.249999999999999112, 5.812500000000000888, -4.846194077712558723 ) ) ;
#2654 = APPROVAL ( #3464, 'UNSPECIFIED' ) ;
#2655 = CARTESIAN_POINT ( 'NONE',  ( -3.749999999999999556, 11.18749999999999822, -1.946699141100892927 ) ) ;
#2656 = CIRCLE ( 'NONE', #13277, 8.000000000000007105 ) ;
#2657 = CARTESIAN_POINT ( 'NONE',  ( -64.42669704464265124, 15.00000000000000000, -184.3342360300873679 ) ) ;
#2658 = CARTESIAN_POINT ( 'NONE',  ( 1.320501113854931408, 5.000000000000000888, -137.8664870916819893 ) ) ;
#2659 = CARTESIAN_POINT ( 'NONE',  ( 2.298097038856279362, 8.875000000000001776, -1.201902961143720860 ) ) ;
#2660 = PERSON_AND_ORGANIZATION_ROLE ( 'classification_officer' ) ;
#2661 = CARTESIAN_POINT ( 'NONE',  ( -1.445049718557150253, 5.000000000000792255, -134.5128495240823270 ) ) ;
#2662 = CARTESIAN_POINT ( 'NONE',  ( 3.364081176287436303, 8.673617379884035472E-16, -112.2881015945827130 ) ) ;
#2663 = VERTEX_POINT ( 'NONE', #8766 ) ;
#2664 = CARTESIAN_POINT ( 'NONE',  ( -3.647146582612662336, 14.99999999999999645, -103.6739734567058662 ) ) ;
#2665 = CARTESIAN_POINT ( 'NONE',  ( 1.500000000000000000, 4.500000000000000888, -0.2499999999999997780 ) ) ;
#2666 = ORIENTED_EDGE ( 'NONE', *, *, #9993, .T. ) ;
#2667 = EDGE_LOOP ( 'NONE', ( #14522, #9827, #12242, #13187 ) ) ;
#2668 = CARTESIAN_POINT ( 'NONE',  ( 5.000000000000000888, 5.000000000000000888, -1.663700395152567513 ) ) ;
#2669 = CARTESIAN_POINT ( 'NONE',  ( -3.750000000000000000, 12.81250000000000178, -5.053300858899105741 ) ) ;
#2670 = CARTESIAN_POINT ( 'NONE',  ( -1.346194077712558945, 10.56250000000000355, -0.2500000000000002220 ) ) ;
#2671 = CARTESIAN_POINT ( 'NONE',  ( 3.249999999999998224, 9.312500000000000000, -2.153805922287439945 ) ) ;
#2672 = EDGE_LOOP ( 'NONE', ( #6989, #928, #356, #3266, #10511, #480, #13102, #13966, #3596, #9914, #5894, #9381, #9465, #2118, #3005, #7630, #5393, #2799 ) ) ;
#2673 = PLANE ( 'NONE',  #10955 ) ;
#2674 = CARTESIAN_POINT ( 'NONE',  ( 3.249999999999999556, 6.750000000000000000, -3.500000000000000000 ) ) ;
#2675 = CARTESIAN_POINT ( 'NONE',  ( -6.848205146710602875, 0.003927834388024460492, -104.1625534234818673 ) ) ;
#2676 = CARTESIAN_POINT ( 'NONE',  ( -42.38382697495404017, 9.999999999999996447, -158.4544082798614397 ) ) ;
#2677 = EDGE_CURVE ( 'NONE', #9805, #5143, #771, .T. ) ;
#2678 = CARTESIAN_POINT ( 'NONE',  ( -58.06539719015423628, 14.99999999999999822, -167.9715705546709614 ) ) ;
#2679 = APPROVAL_DATE_TIME ( #14359, #6787 ) ;
#2680 = DIRECTION ( 'NONE',  ( -0.000000000000000000, -1.000000000000000000, -0.000000000000000000 ) ) ;
#2681 = ORIENTED_EDGE ( 'NONE', *, *, #2219, .F. ) ;
#2682 = CARTESIAN_POINT ( 'NONE',  ( -2.298097038856278473, 1.125000000000000222, -1.201902961143720416 ) ) ;
#2683 = CARTESIAN_POINT ( 'NONE',  ( -3.749999999999999556, 14.31250000000000000, -5.053300858899104853 ) ) ;
#2684 = CARTESIAN_POINT ( 'NONE',  ( -2.157807494669262027, 1.750000000000239142, -0.2731155010785480952 ) ) ;
#2685 = CARTESIAN_POINT ( 'NONE',  ( -3.750000000000000000, 13.81250000000000178, -5.053300858899105741 ) ) ;
#2686 = CIRCLE ( 'NONE', #11805, 2.000000000000000000 ) ;
#2687 = CARTESIAN_POINT ( 'NONE',  ( -63.68606942785788760, 12.31334483161724336, -202.4826902647699001 ) ) ;
#2688 = DIRECTION ( 'NONE',  ( 0.9999958530058989936, 0.000000000000000000, -0.002879925520667555271 ) ) ;
#2689 = CARTESIAN_POINT ( 'NONE',  ( -3.249999999999999556, 2.750000000000000444, -3.500000000000000000 ) ) ;
#2690 = CARTESIAN_POINT ( 'NONE',  ( 10.05365188728890935, 14.67691136496379123, -106.1318723917360671 ) ) ;
#2691 = SECURITY_CLASSIFICATION_LEVEL ( 'unclassified' ) ;
#2692 = EDGE_CURVE ( 'NONE', #12952, #13724, #5360, .T. ) ;
#2693 = CARTESIAN_POINT ( 'NONE',  ( 6.089666224640344794, 0.000000000000000000, -124.6062682140657074 ) ) ;
#2694 = DIRECTION ( 'NONE',  ( -0.9961255586397056438, -0.000000000000000000, 0.08794243244722427244 ) ) ;
#2695 = VERTEX_POINT ( 'NONE', #14811 ) ;
#2696 = CARTESIAN_POINT ( 'NONE',  ( 4.534579168377672609, -0.0002385848209785603532, -1.093758300940373074 ) ) ;
#2697 = CARTESIAN_POINT ( 'NONE',  ( -3.980102097228897245E-16, 5.500000000000000000, -6.749999999999999112 ) ) ;
#2698 = CARTESIAN_POINT ( 'NONE',  ( -69.01969303127702915, 10.00000000000000000, -181.6796560542968848 ) ) ;
#2699 = CARTESIAN_POINT ( 'NONE',  ( 2.298097038856279362, 11.87500000000000000, -1.201902961143720860 ) ) ;
#2700 = CARTESIAN_POINT ( 'NONE',  ( -1.346194077712559167, 9.937500000000001776, -6.749999999999999112 ) ) ;
#2701 = CARTESIAN_POINT ( 'NONE',  ( -4.773065440008094740, 15.00000000000000000, -102.4756705383327073 ) ) ;
#2702 = DIRECTION ( 'NONE',  ( -1.000000000000000000, -0.000000000000000000, -0.000000000000000000 ) ) ;
#2703 = CARTESIAN_POINT ( 'NONE',  ( 9.127846621026490581, 15.00000000000139622, -105.9353198608211670 ) ) ;
#2704 = CARTESIAN_POINT ( 'NONE',  ( 1.346194077712558057, 5.562500000000000000, -6.750000000000000000 ) ) ;
#2705 = CARTESIAN_POINT ( 'NONE',  ( 1.346194077712561166, 15.43750000000000178, -0.2500000000000011102 ) ) ;
#2706 = CARTESIAN_POINT ( 'NONE',  ( -2.651650429449552870, 7.125000000000000000, -0.8483495705504462414 ) ) ;
#2707 = CARTESIAN_POINT ( 'NONE',  ( -3.837140252011802311, 11.25564743829991343, -45.28537430115928686 ) ) ;
#2708 = CARTESIAN_POINT ( 'NONE',  ( -2.651650429449553314, 5.875000000000001776, -6.151650429449552426 ) ) ;
#2709 = CARTESIAN_POINT ( 'NONE',  ( 2.569439577807433928, 14.37659876732869257, 3.184003491651386408 ) ) ;
#2710 = CARTESIAN_POINT ( 'NONE',  ( 0.000000000000000000, 1.750000000000000000, 0.000000000000000000 ) ) ;
#2711 = EDGE_CURVE ( 'NONE', #2289, #5560, #9403, .T. ) ;
#2712 = EDGE_CURVE ( 'NONE', #15113, #5809, #26, .T. ) ;
#2713 = CARTESIAN_POINT ( 'NONE',  ( 30.90149453746306207, 8.773889247172311556, -41.17582585713872589 ) ) ;
#2714 = EDGE_CURVE ( 'NONE', #13895, #5120, #1998, .T. ) ;
#2715 = LINE ( 'NONE', #3877, #9488 ) ;
#2716 = DIRECTION ( 'NONE',  ( 0.000000000000000000, 0.000000000000000000, 1.000000000000000000 ) ) ;
#2717 = CARTESIAN_POINT ( 'NONE',  ( -20.78509463529371004, 8.673617379884033500E-16, -172.2980575345146974 ) ) ;
#2718 = EDGE_LOOP ( 'NONE', ( #6691, #8467, #1302, #11751, #12754 ) ) ;
#2719 = LOCAL_TIME ( 12, 28, 20.00000000000000000, #7464 ) ;
#2720 = CARTESIAN_POINT ( 'NONE',  ( 3.749999999999999112, 12.18750000000000178, -5.053300858899108405 ) ) ;
#2721 = VERTEX_POINT ( 'NONE', #12311 ) ;
#2722 = CARTESIAN_POINT ( 'NONE',  ( -5.145745206871998434, 2.500000000000000444, -112.5500021907323713 ) ) ;
#2723 = CARTESIAN_POINT ( 'NONE',  ( -27.15694708024977189, 8.673617379884035472E-16, -202.7147527119508368 ) ) ;
#2724 = CARTESIAN_POINT ( 'NONE',  ( 3.750000000000000000, 8.750000000000000000, -3.500000000000000444 ) ) ;
#2725 = CARTESIAN_POINT ( 'NONE',  ( -3.750000000000000000, 7.812500000000000000, -5.053300858899105741 ) ) ;
#2726 = AXIS2_PLACEMENT_3D ( 'NONE', #15205, #3280, #7845 ) ;
#2727 = DIRECTION ( 'NONE',  ( 1.224646799147353207E-16, 1.000000000000000000, -0.000000000000000000 ) ) ;
#2728 = EDGE_LOOP ( 'NONE', ( #13599, #1224, #3776 ) ) ;
#2729 = CARTESIAN_POINT ( 'NONE',  ( -3.980102097228897738E-16, 5.999999999999999112, -6.749999999999999112 ) ) ;
#2730 = CARTESIAN_POINT ( 'NONE',  ( 3.750000000000000000, 8.750000000000000000, -3.500000000000000444 ) ) ;
#2731 = CARTESIAN_POINT ( 'NONE',  ( -63.65634297892059124, 15.00000000000000000, -180.4413320423983293 ) ) ;
#2732 = CC_DESIGN_SECURITY_CLASSIFICATION ( #9134, ( #15321 ) ) ;
#2733 = DIRECTION ( 'NONE',  ( -0.9961255586397049777, -0.000000000000000000, 0.08794243244723005948 ) ) ;
#2734 = CIRCLE ( 'NONE', #2986, 5.000000000000004441 ) ;
#2735 = CARTESIAN_POINT ( 'NONE',  ( 3.249999999999999112, 6.812500000000000000, -2.153805922287439945 ) ) ;
#2736 = VECTOR ( 'NONE', #12235, 1000.000000000000227 ) ;
#2737 = EDGE_CURVE ( 'NONE', #698, #7183, #9774, .T. ) ;
#2738 = CARTESIAN_POINT ( 'NONE',  ( -6.338840459429284202, 14.99999999995480060, -126.0591383733374329 ) ) ;
#2739 = CALENDAR_DATE ( 2026, 8, 10 ) ;
#2740 = CIRCLE ( 'NONE', #12358, 5.000000000000000000 ) ;
#2741 = CARTESIAN_POINT ( 'NONE',  ( 2.616643680530136962, -8.673617379884035472E-16, -131.5934110696268249 ) ) ;
#2742 = CARTESIAN_POINT ( 'NONE',  ( 8.322646197883424080, 5.000000000000000888, -114.4990917221399798 ) ) ;
#2743 = VERTEX_POINT ( 'NONE', #6522 ) ;
#2744 = CARTESIAN_POINT ( 'NONE',  ( 6.089666224640341241, 9.999999999999998224, -124.6062682140657074 ) ) ;
#2745 = CARTESIAN_POINT ( 'NONE',  ( -17.32624372123753886, 2.500000000000000444, -129.3796757791584753 ) ) ;
#2746 = ORIENTED_EDGE ( 'NONE', *, *, #4845, .F. ) ;
#2747 = ORIENTED_EDGE ( 'NONE', *, *, #15104, .F. ) ;
#2748 = CARTESIAN_POINT ( 'NONE',  ( 27.03835354040193195, 5.000000000000000888, -138.2189567750509980 ) ) ;
#2749 = CARTESIAN_POINT ( 'NONE',  ( -1.553300858899107073, 13.93750000000000000, -7.249999999999999112 ) ) ;
#2750 = CARTESIAN_POINT ( 'NONE',  ( 1.346194077712561166, 10.43750000000000178, -0.2500000000000011102 ) ) ;
#2751 = CARTESIAN_POINT ( 'NONE',  ( -3.249999999999999112, 9.687500000000000000, -2.153805922287440833 ) ) ;
#2752 = ORIENTED_EDGE ( 'NONE', *, *, #2995, .F. ) ;
#2753 = AXIS2_PLACEMENT_3D ( 'NONE', #7559, #4248, #8720 ) ;
#2754 = CARTESIAN_POINT ( 'NONE',  ( -6.310237929021329961, 14.99999999999999822, -119.2996315833885035 ) ) ;
#2755 = VECTOR ( 'NONE', #5893, 1000.000000000000000 ) ;
#2756 = CARTESIAN_POINT ( 'NONE',  ( -3.249999999999999556, 8.250000000000000000, -3.499999999999999556 ) ) ;
#2757 = CIRCLE ( 'NONE', #2990, 1.771449424009387208 ) ;
#2758 = CARTESIAN_POINT ( 'NONE',  ( 9.976451240238549900, 12.67941325565633548, -45.12530232831228716 ) ) ;
#2759 = CARTESIAN_POINT ( 'NONE',  ( -49.14320000630262086, 10.00000000000000178, -164.0715453079124870 ) ) ;
#2760 = CARTESIAN_POINT ( 'NONE',  ( -59.60145741454977752, 14.99999999999999645, -170.6931484237352379 ) ) ;
#2761 = PERSON_AND_ORGANIZATION_ROLE ( 'classification_officer' ) ;
#2762 = CIRCLE ( 'NONE', #2498, 1.000000000000000888 ) ;
#2763 = ORIENTED_EDGE ( 'NONE', *, *, #7781, .F. ) ;
#2764 = CARTESIAN_POINT ( 'NONE',  ( 3.249999999999998668, 0.6875000000000000000, -4.846194077712560500 ) ) ;
#2765 = CARTESIAN_POINT ( 'NONE',  ( -2.651650429449553314, 12.37500000000000000, -6.151650429449552426 ) ) ;
#2766 = DIRECTION ( 'NONE',  ( 0.000000000000000000, 0.000000000000000000, -1.000000000000000000 ) ) ;
#2767 = VECTOR ( 'NONE', #6241, 1000.000000000000000 ) ;
#2768 = CARTESIAN_POINT ( 'NONE',  ( -4.592425496802573972E-16, 0.5000000000000000000, -7.249999999999999112 ) ) ;
#2769 = CARTESIAN_POINT ( 'NONE',  ( -63.24804750230908468, 10.63074368444023676, -203.5304119779587211 ) ) ;
#2770 = FACE_OUTER_BOUND ( 'NONE', #5899, .T. ) ;
#2771 = CARTESIAN_POINT ( 'NONE',  ( 10.88592809031993092, 3.654497976000929516, -107.0374611167700607 ) ) ;
#2772 = DATE_TIME_ROLE ( 'creation_date' ) ;
#2773 = CARTESIAN_POINT ( 'NONE',  ( -67.63291399244498336, 12.29434701114028705, -203.1533042379604979 ) ) ;
#2774 = CARTESIAN_POINT ( 'NONE',  ( 14.22910372453204353, 12.49999999999999822, -126.5134921567817941 ) ) ;
#2775 = APPROVAL_PERSON_ORGANIZATION ( #3973, #2249, #9995 ) ;
#2776 = VERTEX_POINT ( 'NONE', #9925 ) ;
#2777 = CARTESIAN_POINT ( 'NONE',  ( 5.018427371053902242, 0.04004715687429680204, 0.6822673155829361846 ) ) ;
#2778 = CARTESIAN_POINT ( 'NONE',  ( 2.298097038856278473, 7.625000000000000000, -5.798097038856279362 ) ) ;
#2779 = CARTESIAN_POINT ( 'NONE',  ( -9.240119717576689595, 2.500000000000000444, -104.6630069175297564 ) ) ;
#2780 = CARTESIAN_POINT ( 'NONE',  ( -3.980102097228897245E-16, 12.50000000000000000, -6.749999999999999112 ) ) ;
#2781 = EDGE_CURVE ( 'NONE', #933, #14561, #1007, .T. ) ;
#2782 = CARTESIAN_POINT ( 'NONE',  ( 3.249999999999998224, 10.18750000000000533, -4.846194077712561388 ) ) ;
#2783 = DIRECTION ( 'NONE',  ( -0.08794243244722428632, -0.000000000000000000, -0.9961255586397056438 ) ) ;
#2784 = FACE_OUTER_BOUND ( 'NONE', #4308, .T. ) ;
#2785 = FACE_OUTER_BOUND ( 'NONE', #12166, .T. ) ;
#2786 = EDGE_CURVE ( 'NONE', #14187, #10636, #6901, .T. ) ;
#2787 = CARTESIAN_POINT ( 'NONE',  ( -3.249999999999999556, 4.312500000000000888, -4.846194077712557835 ) ) ;
#2788 = CARTESIAN_POINT ( 'NONE',  ( -3.750000000000000000, 4.687500000000000000, -1.946699141100893149 ) ) ;
#2789 = CARTESIAN_POINT ( 'NONE',  ( 3.750000000000000000, 10.75000000000000000, -3.500000000000000444 ) ) ;
#2790 = CARTESIAN_POINT ( 'NONE',  ( -3.330734844456505694, 10.45935787353785074, -44.51265823977242775 ) ) ;
#2791 = CARTESIAN_POINT ( 'NONE',  ( -4.592425496802573972E-16, 7.000000000000000000, -7.250000000000000000 ) ) ;
#2792 = CARTESIAN_POINT ( 'NONE',  ( 3.568580374889821272, 12.24296972320970944, 4.586805082927478239 ) ) ;
#2793 = CARTESIAN_POINT ( 'NONE',  ( 7.352489943804306094, -2.529993217055220178, -39.38380306805897391 ) ) ;
#2794 = VECTOR ( 'NONE', #57, 1000.000000000000227 ) ;
#2795 = CARTESIAN_POINT ( 'NONE',  ( 8.394286649619360219, 0.4947992169189873168, -105.8820645551709418 ) ) ;
#2796 = CARTESIAN_POINT ( 'NONE',  ( -76.20282042307043469, 5.000000000000000000, -188.4633497277648928 ) ) ;
#2797 = CARTESIAN_POINT ( 'NONE',  ( 5.592744633116710773, 0.02476476750516211703, -140.8472914376584981 ) ) ;
#2798 = CARTESIAN_POINT ( 'NONE',  ( -16.95575562637076317, 8.673617379884034486E-16, -165.1048961890580244 ) ) ;
#2799 = ORIENTED_EDGE ( 'NONE', *, *, #1088, .F. ) ;
#2800 = CARTESIAN_POINT ( 'NONE',  ( 1.553300858899105963, 14.06250000000000178, -7.250000000000000888 ) ) ;
#2801 = VERTEX_POINT ( 'NONE', #12244 ) ;
#2802 = DIRECTION ( 'NONE',  ( -0.08794243244722413366, 0.000000000000000000, -0.9961255586397056438 ) ) ;
#2803 = CARTESIAN_POINT ( 'NONE',  ( -20.53214307163321450, 4.000000000000000000, -200.7518619190079505 ) ) ;
#2804 = CARTESIAN_POINT ( 'NONE',  ( -1.553300858899106629, 8.062500000000000000, 0.2500000000000002220 ) ) ;
#2805 = CARTESIAN_POINT ( 'NONE',  ( 3.749999999999998668, 7.187500000000000888, -5.053300858899108405 ) ) ;
#2806 = CARTESIAN_POINT ( 'NONE',  ( 0.2499999999999999445, 4.500000000000000888, -0.2499999999999997780 ) ) ;
#2807 = VERTEX_POINT ( 'NONE', #13421 ) ;
#2808 = EDGE_CURVE ( 'NONE', #5961, #12717, #5292, .T. ) ;
#2809 = CARTESIAN_POINT ( 'NONE',  ( -9.392097536374029332, 3.253592935916376216, -116.4406435548291796 ) ) ;
#2810 = ADVANCED_BREP_SHAPE_REPRESENTATION ( '', ( #7115, #9419 ), #6710 ) ;
#2811 = CARTESIAN_POINT ( 'NONE',  ( -1.346194077712558945, 4.562500000000000000, -0.2500000000000002220 ) ) ;
#2812 = EDGE_CURVE ( 'NONE', #922, #6135, #10003, .T. ) ;
#2813 = CARTESIAN_POINT ( 'NONE',  ( -4.592425496802573972E-16, 9.500000000000000000, -7.249999999999999112 ) ) ;
#2814 = CARTESIAN_POINT ( 'NONE',  ( -70.02757949906018098, 9.999999999999998224, -189.2441461653057218 ) ) ;
#2815 = CARTESIAN_POINT ( 'NONE',  ( -3.806220192786536671, 7.379999999999995453, -48.79866403991030666 ) ) ;
#2816 = APPROVAL_DATE_TIME ( #417, #2249 ) ;
#2817 = CARTESIAN_POINT ( 'NONE',  ( -2.298097038856278918, 9.375000000000000000, -5.798097038856277585 ) ) ;
#2818 = CARTESIAN_POINT ( 'NONE',  ( -9.492276965212552042, 15.00000000002442491, -117.3221826542650490 ) ) ;
#2819 = CARTESIAN_POINT ( 'NONE',  ( -8.326762665057291457, 4.999999999999208633, -121.0857513973247279 ) ) ;
#2820 = CARTESIAN_POINT ( 'NONE',  ( 8.873074003812353894, 5.000000000000000888, -110.5883967389741827 ) ) ;
#2821 = ORIENTED_EDGE ( 'NONE', *, *, #3761, .T. ) ;
#2822 = AXIS2_PLACEMENT_3D ( 'NONE', #4457, #1983, #9170 ) ;
#2823 = DIRECTION ( 'NONE',  ( 0.000000000000000000, 1.000000000000000000, 0.000000000000000000 ) ) ;
#2824 = AXIS2_PLACEMENT_3D ( 'NONE', #8319, #7389, #1450 ) ;
#2825 = CARTESIAN_POINT ( 'NONE',  ( 4.999922846598173543, 0.03155975272377924828, -16.26256187091226835 ) ) ;
#2826 = VERTEX_POINT ( 'NONE', #6367 ) ;
#2827 = DIRECTION ( 'NONE',  ( 0.000000000000000000, 0.000000000000000000, -1.000000000000000000 ) ) ;
#2828 = CARTESIAN_POINT ( 'NONE',  ( 20.87131526946579285, 0.000000000000000000, -138.9752963459259547 ) ) ;
#2829 =( BOUNDED_SURFACE ( )  B_SPLINE_SURFACE ( 3, 2, ( 
 ( #12532, #15101, #3033 ),
 ( #1946, #12460, #6659 ),
 ( #1878, #9056, #7887 ),
 ( #12610, #11450, #870 ),
 ( #4415, #5797, #11595 ),
 ( #8040, #2476, #8336 ),
 ( #2252, #6879, #11674 ),
 ( #9352, #9433, #1014 ) ),
 .UNSPECIFIED., .F., .F., .T. ) 
 B_SPLINE_SURFACE_WITH_KNOTS ( ( 4, 2, 2, 4 ),
 ( 3, 3 ),
 ( 0.06905721847989758355, 0.07704657673304832199, 0.08503593498619907431, 0.1010146514925005512 ),
 ( 0.000000000000000000, 1.000000000000000000 ),
 .UNSPECIFIED. ) 
 GEOMETRIC_REPRESENTATION_ITEM ( )  RATIONAL_B_SPLINE_SURFACE ( (
 ( 1.000000000000000000, 0.7071067811865475727, 1.000000000000000000),
 ( 1.000000000000000000, 0.7071067811865475727, 1.000000000000000000),
 ( 1.000000000000000000, 0.7071067811865475727, 1.000000000000000000),
 ( 1.000000000000000000, 0.7071067811865475727, 1.000000000000000000),
 ( 1.000000000000000000, 0.7071067811865473507, 1.000000000000000000),
 ( 1.000000000000000000, 0.7071067811865473507, 1.000000000000000000),
 ( 1.000000000000000000, 0.7071067811865475727, 1.000000000000000000),
 ( 1.000000000000000000, 0.7071067811865475727, 1.000000000000000000) ) ) 
 REPRESENTATION_ITEM ( '' )  SURFACE ( )  );
#2830 = CARTESIAN_POINT ( 'NONE',  ( -2.651650429449552870, 13.87500000000000178, -6.151650429449552426 ) ) ;
#2831 = CARTESIAN_POINT ( 'NONE',  ( 2.298097038856278029, 13.12500000000000178, -5.798097038856279362 ) ) ;
#2832 = CARTESIAN_POINT ( 'NONE',  ( 1.346194077712561166, 10.43750000000000178, -0.2500000000000011102 ) ) ;
#2833 = ORIENTED_EDGE ( 'NONE', *, *, #15271, .F. ) ;
#2834 = DIRECTION ( 'NONE',  ( 0.6527336816407247611, 0.000000000000000000, -0.7575874476598360996 ) ) ;
#2835 = CARTESIAN_POINT ( 'NONE',  ( 1.346194077712558057, 8.562500000000001776, -6.750000000000000000 ) ) ;
#2836 = EDGE_CURVE ( 'NONE', #4737, #6769, #13190, .T. ) ;
#2837 = VECTOR ( 'NONE', #4354, 1000.000000000000000 ) ;
#2838 = CARTESIAN_POINT ( 'NONE',  ( 1.013023623609336843, 4.588323854676484181, -139.4901577088605791 ) ) ;
#2839 = CARTESIAN_POINT ( 'NONE',  ( 1.004809442601927394, 5.000000000000000888, -139.4752805618705622 ) ) ;
#2840 = DIRECTION ( 'NONE',  ( 0.9961255586397056438, 0.000000000000000000, -0.08794243244722427244 ) ) ;
#2841 = DIRECTION ( 'NONE',  ( 0.000000000000000000, 1.000000000000000000, 0.000000000000000000 ) ) ;
#2842 = APPROVAL_STATUS ( 'not_yet_approved' ) ;
#2843 = LINE ( 'NONE', #12327, #13451 ) ;
#2844 = ORIENTED_EDGE ( 'NONE', *, *, #12794, .F. ) ;
#2845 = CARTESIAN_POINT ( 'NONE',  ( -1.346194077712559389, 2.062500000000000000, -0.2500000000000002220 ) ) ;
#2846 = CIRCLE ( 'NONE', #8761, 3.000000000000011990 ) ;
#2847 = CARTESIAN_POINT ( 'NONE',  ( -2.651650429449552870, 14.12500000000000000, -0.8483495705504462414 ) ) ;
#2848 = ORIENTED_EDGE ( 'NONE', *, *, #7527, .F. ) ;
#2849 = DIRECTION ( 'NONE',  ( -0.000000000000000000, -1.000000000000000000, -0.000000000000000000 ) ) ;
#2850 = CARTESIAN_POINT ( 'NONE',  ( -3.749999999999999556, 0.3125000000000000555, -5.053300858899104853 ) ) ;
#2851 = CARTESIAN_POINT ( 'NONE',  ( 7.740440778602579286, 4.463770477647834412, -20.78498225277660083 ) ) ;
#2852 = CARTESIAN_POINT ( 'NONE',  ( 14.22910372453204353, 12.49999999999999822, -126.5134921567817941 ) ) ;
#2853 = CARTESIAN_POINT ( 'NONE',  ( -2.651650429449553314, 0.3750000000000000555, -6.151650429449552426 ) ) ;
#2854 = APPLICATION_PROTOCOL_DEFINITION ( 'international standard', 'config_control_design', 1994, #8173 ) ;
#2855 = CARTESIAN_POINT ( 'NONE',  ( -67.60484011711940866, 11.30829572562506335, -204.1139660933697257 ) ) ;
#2856 = CARTESIAN_POINT ( 'NONE',  ( 11.04730217088347644, 5.000000000000000888, -107.1178495010082656 ) ) ;
#2857 = ORIENTED_EDGE ( 'NONE', *, *, #8813, .F. ) ;
#2858 = CARTESIAN_POINT ( 'NONE',  ( 3.249999999999998668, 8.687500000000000000, -4.846194077712560500 ) ) ;
#2859 = DIRECTION ( 'NONE',  ( 0.000000000000000000, 1.000000000000000000, 0.000000000000000000 ) ) ;
#2860 = CARTESIAN_POINT ( 'NONE',  ( 1.346194077712560944, 14.93750000000000178, -0.2500000000000010547 ) ) ;
#2861 = CARTESIAN_POINT ( 'NONE',  ( -1.346194077712559167, 8.937500000000000000, -6.749999999999999112 ) ) ;
#2862 = CARTESIAN_POINT ( 'NONE',  ( -2.573490212646732278, 7.321094445766561876, -29.14997122992682321 ) ) ;
#2863 = CARTESIAN_POINT ( 'NONE',  ( 51.16773099383375012, 8.094429697821059805E-15, 70.62880098866565959 ) ) ;
#2864 = CARTESIAN_POINT ( 'NONE',  ( -10.46704385831657902, 4.336808689942017736E-16, -128.9524512386204549 ) ) ;
#2865 = CARTESIAN_POINT ( 'NONE',  ( 1.346194077712558057, 6.562500000000000000, -6.750000000000000000 ) ) ;
#2866 = CARTESIAN_POINT ( 'NONE',  ( -2.651650429449552870, 4.875000000000000000, -6.151650429449552426 ) ) ;
#2867 = CARTESIAN_POINT ( 'NONE',  ( -2.651650429449552870, 10.12500000000000000, -0.8483495705504462414 ) ) ;
#2868 = FACE_BOUND ( 'NONE', #8635, .T. ) ;
#2869 = CARTESIAN_POINT ( 'NONE',  ( 0.2343396196498212236, 3.734791725217455394, 2.654369205397980380 ) ) ;
#2870 = CARTESIAN_POINT ( 'NONE',  ( 1.553300858899109516, 11.43750000000000178, 0.2499999999999993616 ) ) ;
#2871 = CARTESIAN_POINT ( 'NONE',  ( -6.683304552674626642, 0.000000000000000000, -104.1296019027811894 ) ) ;
#2872 = CARTESIAN_POINT ( 'NONE',  ( 10.00185261163550976, 0.09491738922320896998, -163.8759456858575163 ) ) ;
#2873 = CARTESIAN_POINT ( 'NONE',  ( 1.990297875723448406, 0.000000000000000000, 3.483276348926833244 ) ) ;
#2874 = CARTESIAN_POINT ( 'NONE',  ( -12.11204790299879086, 8.673617379884035472E-16, -158.0701594236071514 ) ) ;
#2875 = CARTESIAN_POINT ( 'NONE',  ( -0.3766621274091713767, 0.2975415354274087432, -7.146945437571386783 ) ) ;
#2876 = CARTESIAN_POINT ( 'NONE',  ( -0.8029028047895949705, 8.673617379884034486E-16, -146.7767709142194121 ) ) ;
#2877 = CARTESIAN_POINT ( 'NONE',  ( 1.346194077712558279, 0.06250000000000016653, -6.750000000000000888 ) ) ;
#2878 = ORIENTED_EDGE ( 'NONE', *, *, #13294, .F. ) ;
#2879 = DIRECTION ( 'NONE',  ( -0.8645818496218652394, 0.000000000000000000, 0.5024920151648527566 ) ) ;
#2880 = CARTESIAN_POINT ( 'NONE',  ( 2.651650429449552870, 7.625000000000000000, -6.151650429449554203 ) ) ;
#2881 = CARTESIAN_POINT ( 'NONE',  ( 1.553300858899105963, 10.06250000000000000, -7.249999999999999112 ) ) ;
#2882 = CARTESIAN_POINT ( 'NONE',  ( 26.88777289245747326, 6.000000000000000000, -138.4814624290440577 ) ) ;
#2883 = ORIENTED_EDGE ( 'NONE', *, *, #13980, .T. ) ;
#2884 = CARTESIAN_POINT ( 'NONE',  ( -3.249999999999999112, 7.812500000000000000, -4.846194077712558723 ) ) ;
#2885 = CARTESIAN_POINT ( 'NONE',  ( -3.750000000000000000, 13.25000000000000000, -3.499999999999999112 ) ) ;
#2886 = DIRECTION ( 'NONE',  ( 1.000000000000000000, 0.000000000000000000, 0.000000000000000000 ) ) ;
#2887 = CARTESIAN_POINT ( 'NONE',  ( -4.492499072540820926, 0.000000000000000000, 2.611025101989610686 ) ) ;
#2888 = APPLICATION_PROTOCOL_DEFINITION ( 'international standard', 'config_control_design', 1994, #14617 ) ;
#2889 = CARTESIAN_POINT ( 'NONE',  ( 1.346194077712558057, 10.56250000000000000, -6.750000000000000000 ) ) ;
#2890 = CARTESIAN_POINT ( 'NONE',  ( 8.131300352726237080, 2.490287375297123962, -39.89901737624450107 ) ) ;
#2891 = EDGE_CURVE ( 'NONE', #10548, #4391, #5215, .T. ) ;
#2892 = CARTESIAN_POINT ( 'NONE',  ( -9.518035003875171540, 4.999999999998426148, -117.2217326885085669 ) ) ;
#2893 = CARTESIAN_POINT ( 'NONE',  ( 10.69730027799064764, -3.493608200715386290E-11, -107.4734661196424241 ) ) ;
#2894 = DIRECTION ( 'NONE',  ( 1.000000000000000000, 0.000000000000000000, 0.000000000000000000 ) ) ;
#2895 = CARTESIAN_POINT ( 'NONE',  ( 10.97120727310200472, 11.75624639942191507, -44.98549499369563165 ) ) ;
#2896 = VERTEX_POINT ( 'NONE', #2745 ) ;
#2897 = CARTESIAN_POINT ( 'NONE',  ( 9.958478854730328678, 4.811568727942957757, -44.17880315911963862 ) ) ;
#2898 = DIRECTION ( 'NONE',  ( 0.9026204165532970558, 0.000000000000000000, 0.4304374328763155289 ) ) ;
#2899 = CARTESIAN_POINT ( 'NONE',  ( -2.651650429449552870, 13.62500000000000000, -0.8483495705504467965 ) ) ;
#2900 = CARTESIAN_POINT ( 'NONE',  ( -3.249999999999999112, 10.68750000000000178, -2.153805922287440833 ) ) ;
#2901 = CARTESIAN_POINT ( 'NONE',  ( -2.298097038856279362, 12.87500000000000000, -5.798097038856278473 ) ) ;
#2902 = ORIENTED_EDGE ( 'NONE', *, *, #14787, .T. ) ;
#2903 = CARTESIAN_POINT ( 'NONE',  ( -3.249999999999999556, 9.187500000000000000, -2.153805922287440833 ) ) ;
#2904 = FACE_OUTER_BOUND ( 'NONE', #15245, .T. ) ;
#2905 = CARTESIAN_POINT ( 'NONE',  ( -6.530393906344411192, 14.42323828349428361, -104.0689525186695477 ) ) ;
#2906 = DIRECTION ( 'NONE',  ( 0.000000000000000000, 1.000000000000000000, 0.000000000000000000 ) ) ;
#2907 = CARTESIAN_POINT ( 'NONE',  ( -9.625715240929997307, 11.51017254279852509, -115.8367759348243595 ) ) ;
#2908 = APPLICATION_PROTOCOL_DEFINITION ( 'international standard', 'config_control_design', 1994, #12731 ) ;
#2909 = EDGE_CURVE ( 'NONE', #2518, #11832, #8887, .T. ) ;
#2910 = DIRECTION ( 'NONE',  ( 0.08794243244722392550, 0.000000000000000000, 0.9961255586397055328 ) ) ;
#2911 =( BOUNDED_CURVE ( )  B_SPLINE_CURVE ( 3, ( #669, #593, #5375, #10018 ),
 .UNSPECIFIED., .F., .T. ) 
 B_SPLINE_CURVE_WITH_KNOTS ( ( 4, 4 ),
 ( 4.702026407136986386, 4.709001436419505637 ),
 .UNSPECIFIED. ) 
 CURVE ( )  GEOMETRIC_REPRESENTATION_ITEM ( )  RATIONAL_B_SPLINE_CURVE ( ( 1.000000000000000000, 0.9999959457513183381, 0.9999959457513183381, 1.000000000000000000 ) ) 
 REPRESENTATION_ITEM ( '' )  );
#2912 = ADVANCED_FACE ( 'NONE', ( #11011 ), #14581, .T. ) ;
#2913 = EDGE_CURVE ( 'NONE', #2651, #5826, #4357, .T. ) ;
#2914 = ORIENTED_EDGE ( 'NONE', *, *, #981, .T. ) ;
#2915 = CARTESIAN_POINT ( 'NONE',  ( -2.298097038856278029, 13.62500000000000000, -1.201902961143720638 ) ) ;
#2916 = CARTESIAN_POINT ( 'NONE',  ( -1.553300858899106629, 14.06249999999999822, 0.2500000000000002220 ) ) ;
#2917 = EDGE_LOOP ( 'NONE', ( #3608, #10118 ) ) ;
#2918 = DIRECTION ( 'NONE',  ( 0.000000000000000000, 1.000000000000000000, 0.000000000000000000 ) ) ;
#2919 = CARTESIAN_POINT ( 'NONE',  ( -4.592425496802573972E-16, 1.500000000000000000, -7.249999999999999112 ) ) ;
#2920 = CARTESIAN_POINT ( 'NONE',  ( -25.68053481550299111, 5.000000000000000888, -142.4798935003980773 ) ) ;
#2921 = CARTESIAN_POINT ( 'NONE',  ( 3.087044391538636745, 1.679853004339140421, 3.965071156515985518 ) ) ;
#2922 = CARTESIAN_POINT ( 'NONE',  ( -3.750000000000000000, 1.187500000000000000, -1.946699141100892927 ) ) ;
#2923 = APPROVAL_STATUS ( 'not_yet_approved' ) ;
#2924 = CARTESIAN_POINT ( 'NONE',  ( -67.56452796570999908, 13.67829370444025372, -200.1615161516820365 ) ) ;
#2925 = CARTESIAN_POINT ( 'NONE',  ( 26.71007981443201018, 12.49999999999999822, -136.8791680534710054 ) ) ;
#2926 = ORIENTED_EDGE ( 'NONE', *, *, #13361, .T. ) ;
#2927 = CARTESIAN_POINT ( 'NONE',  ( 1.346194077712560944, 9.937499999999998224, -0.2500000000000011102 ) ) ;
#2928 = APPROVAL ( #1843, 'UNSPECIFIED' ) ;
#2929 = DIRECTION ( 'NONE',  ( -1.000000000000000000, 0.000000000000000000, -0.000000000000000000 ) ) ;
#2930 = CARTESIAN_POINT ( 'NONE',  ( 3.249999999999998224, 2.312500000000000000, -2.153805922287439945 ) ) ;
#2931 = CARTESIAN_POINT ( 'NONE',  ( 0.000000000000000000, 12.50000000000000178, -0.2500000000000002220 ) ) ;
#2932 = CARTESIAN_POINT ( 'NONE',  ( -3.816819072638210297, 15.00000000000000000, -103.4918378357580053 ) ) ;
#2933 = DIRECTION ( 'NONE',  ( -0.000000000000000000, -1.000000000000000000, -0.000000000000000000 ) ) ;
#2934 = CARTESIAN_POINT ( 'NONE',  ( 1.346194077712560944, 3.937500000000000000, -0.2500000000000010547 ) ) ;
#2935 = CARTESIAN_POINT ( 'NONE',  ( 2.651650429449552870, 4.125000000000000000, -6.151650429449553314 ) ) ;
#2936 = CARTESIAN_POINT ( 'NONE',  ( 1.553300858899108849, 10.93750000000000178, 0.2499999999999993616 ) ) ;
#2937 = CARTESIAN_POINT ( 'NONE',  ( -3.648797883638982054, 2.490287375297123962, -1.000000000000000888 ) ) ;
#2938 = CARTESIAN_POINT ( 'NONE',  ( 0.000000000000000000, 1.000000000000000000, -6.000000000000002665 ) ) ;
#2939 = CARTESIAN_POINT ( 'NONE',  ( -3.749999999999999556, 11.75000000000000178, -3.499999999999999112 ) ) ;
#2940 = CARTESIAN_POINT ( 'NONE',  ( 4.351317386395303188, 0.03165940128134000359, -16.24646476423705010 ) ) ;
#2941 = CARTESIAN_POINT ( 'NONE',  ( 12.85253911111128389, 2.933442265363937818, -165.9654706698083828 ) ) ;
#2942 = DIRECTION ( 'NONE',  ( 0.08794243244723000397, 0.000000000000000000, 0.9961255586397049777 ) ) ;
#2943 = CARTESIAN_POINT ( 'NONE',  ( -25.15812356329616151, -6.561949609624546619E-12, -172.1841440208294784 ) ) ;
#2944 = FACE_OUTER_BOUND ( 'NONE', #3061, .T. ) ;
#2945 = UNCERTAINTY_MEASURE_WITH_UNIT (LENGTH_MEASURE( 1.000000000000000082E-05 ), #13919, 'distance_accuracy_value', 'NONE');
#2946 = CARTESIAN_POINT ( 'NONE',  ( -44.50300032310534704, 15.00000000000000000, -159.8141794072773223 ) ) ;
#2947 = CARTESIAN_POINT ( 'NONE',  ( -2.651650429449553314, 12.87500000000000000, -6.151650429449552426 ) ) ;
#2948 = ORIENTED_EDGE ( 'NONE', *, *, #12150, .F. ) ;
#2949 = FACE_OUTER_BOUND ( 'NONE', #8077, .T. ) ;
#2950 = CARTESIAN_POINT ( 'NONE',  ( 18.69225092093103058, 2.850949024098341860E-47, -142.9045830238807184 ) ) ;
#2951 = CARTESIAN_POINT ( 'NONE',  ( 3.749999999999999556, 7.250000000000000000, -3.500000000000000444 ) ) ;
#2952 = DIRECTION ( 'NONE',  ( 0.000000000000000000, 1.000000000000000000, 0.000000000000000000 ) ) ;
#2953 = CARTESIAN_POINT ( 'NONE',  ( -3.249999999999999112, 6.687500000000000888, -2.153805922287440833 ) ) ;
#2954 = DIRECTION ( 'NONE',  ( 0.000000000000000000, 1.000000000000000000, 0.000000000000000000 ) ) ;
#2955 = CARTESIAN_POINT ( 'NONE',  ( -3.750000000000000000, -0.1874999999999998890, -5.053300858899105741 ) ) ;
#2956 = FACE_OUTER_BOUND ( 'NONE', #12437, .T. ) ;
#2957 = DIRECTION ( 'NONE',  ( 0.000000000000000000, 1.000000000000000000, 0.000000000000000000 ) ) ;
#2958 = CARTESIAN_POINT ( 'NONE',  ( -2.298097038856278918, 10.37500000000000000, -5.798097038856277585 ) ) ;
#2959 = CARTESIAN_POINT ( 'NONE',  ( -5.488578029460351893, 2.075239479414269894, -43.69424231201529096 ) ) ;
#2960 = LOCAL_TIME ( 12, 28, 20.00000000000000000, #13657 ) ;
#2961 = DIRECTION ( 'NONE',  ( -0.02181900108494679719, 0.000000000000000000, 0.9997619372588931741 ) ) ;
#2962 = CARTESIAN_POINT ( 'NONE',  ( 9.247146435675446696, 0.000000000000000000, -109.6962599556842832 ) ) ;
#2963 = AXIS2_PLACEMENT_3D ( 'NONE', #7976, #807, #5508 ) ;
#2964 = CARTESIAN_POINT ( 'NONE',  ( -16.94138229547579400, 5.000000000000000888, -154.2864167784019287 ) ) ;
#2965 = DIRECTION ( 'NONE',  ( 1.000000000000000000, 0.000000000000000000, 0.000000000000000000 ) ) ;
#2966 = ORIENTED_EDGE ( 'NONE', *, *, #7047, .F. ) ;
#2967 = LINE ( 'NONE', #7598, #14009 ) ;
#2968 = CARTESIAN_POINT ( 'NONE',  ( -4.234402844927150689, 15.00000000000000000, -117.4888040839639558 ) ) ;
#2969 = CARTESIAN_POINT ( 'NONE',  ( 0.000000000000000000, 2.000000000000000000, 0.2500000000000002220 ) ) ;
#2970 = CARTESIAN_POINT ( 'NONE',  ( -1.346194077712558945, 9.562500000000000000, -0.2500000000000002220 ) ) ;
#2971 = CARTESIAN_POINT ( 'NONE',  ( -3.980102097228897245E-16, 0.5000000000000000000, -6.749999999999999112 ) ) ;
#2972 = ORIENTED_EDGE ( 'NONE', *, *, #7214, .F. ) ;
#2973 = ADVANCED_FACE ( 'NONE', ( #2263 ), #4576, .F. ) ;
#2974 = EDGE_CURVE ( 'NONE', #14170, #6819, #5582, .T. ) ;
#2975 = CARTESIAN_POINT ( 'NONE',  ( -3.249999999999999556, 10.18750000000000000, -2.153805922287440833 ) ) ;
#2976 = APPROVAL_PERSON_ORGANIZATION ( #6902, #12916, #7991 ) ;
#2977 = ADVANCED_FACE ( 'NONE', ( #3185 ), #2095, .F. ) ;
#2978 = CIRCLE ( 'NONE', #3704, 1.000000000000000888 ) ;
#2979 = CARTESIAN_POINT ( 'NONE',  ( 3.249999999999999112, 8.812500000000000000, -2.153805922287439945 ) ) ;
#2980 = CARTESIAN_POINT ( 'NONE',  ( 4.370967001746241642, 0.4765682694954604393, 1.559350592413775605 ) ) ;
#2981 = DIRECTION ( 'NONE',  ( 0.02181900108494732801, 0.000000000000000000, -0.9997619372588932851 ) ) ;
#2982 = CALENDAR_DATE ( 2026, 8, 10 ) ;
#2983 = CARTESIAN_POINT ( 'NONE',  ( 8.428994341907280585, 15.00000000000046896, -112.3028785388761861 ) ) ;
#2984 = PRODUCT_DEFINITION ( 'UNKNOWN', '', #8443, #8817 ) ;
#2985 = ORIENTED_EDGE ( 'NONE', *, *, #1841, .T. ) ;
#2986 = AXIS2_PLACEMENT_3D ( 'NONE', #7808, #2089, #5490 ) ;
#2987 = CARTESIAN_POINT ( 'NONE',  ( 1.346194077712560944, 5.937500000000000000, -0.2500000000000010547 ) ) ;
#2988 = DIRECTION ( 'NONE',  ( 0.000000000000000000, 0.000000000000000000, -1.000000000000000000 ) ) ;
#2989 = CARTESIAN_POINT ( 'NONE',  ( 0.000000000000000000, 12.00000000000000000, 0.2500000000000002220 ) ) ;
#2990 = AXIS2_PLACEMENT_3D ( 'NONE', #2710, #7413, #7647 ) ;
#2991 = CIRCLE ( 'NONE', #764, 3.000000000000005329 ) ;
#2992 = VERTEX_POINT ( 'NONE', #10374 ) ;
#2993 = EDGE_CURVE ( 'NONE', #6034, #4876, #1378, .T. ) ;
#2994 = CARTESIAN_POINT ( 'NONE',  ( 0.000000000000000000, 3.000000000000000000, 0.2500000000000002220 ) ) ;
#2995 = EDGE_CURVE ( 'NONE', #5143, #15130, #5431, .T. ) ;
#2996 = B_SPLINE_CURVE_WITH_KNOTS ( 'NONE', 3,
 ( #13858, #3110, #7968, #6740, #10224, #5726, #11453, #11376, #4277, #9284, #7821, #800, #5576, #3256, #14008, #5502, #2105, #3406, #8116, #5947 ),
 .UNSPECIFIED., .F., .F.,
 ( 4, 2, 2, 2, 2, 2, 2, 2, 2, 4 ),
 ( -1.586050209718467129E-05, 0.001006126488465763913, 0.002028113479028712755, 0.003050100469591661596, 0.004072087460154610004, 0.005094074450717559280, 0.005605067945999035219, 0.006116061441280511157, 0.007138048431843450892, 0.008160035422406390626 ),
 .UNSPECIFIED. ) ;
#2997 = VECTOR ( 'NONE', #716, 1000.000000000000227 ) ;
#2998 = CARTESIAN_POINT ( 'NONE',  ( 7.190027994173562753, 5.321094445766561876, -30.38850508759179192 ) ) ;
#2999 = CARTESIAN_POINT ( 'NONE',  ( 0.1841197429283822073, 0.1140767794773729221, 2.085527733063581746 ) ) ;
#3000 =( BOUNDED_SURFACE ( )  B_SPLINE_SURFACE ( 3, 2, ( 
 ( #664, #7687, #737 ),
 ( #890, #5442, #10086 ),
 ( #14820, #8924, #6608 ),
 ( #3053, #13651, #12322 ),
 ( #14973, #12479, #5372 ),
 ( #10163, #3194, #7765 ),
 ( #12633, #10241, #1896 ),
 ( #14898, #9149, #4294 ) ),
 .UNSPECIFIED., .F., .F., .F. ) 
 B_SPLINE_SURFACE_WITH_KNOTS ( ( 4, 2, 2, 4 ),
 ( 3, 3 ),
 ( 0.000000000000000000, 0.0007402894036727104788, 0.001480578807345420958, 0.002961157614690841915 ),
 ( 0.000000000000000000, 1.000000000000000000 ),
 .UNSPECIFIED. ) 
 GEOMETRIC_REPRESENTATION_ITEM ( )  RATIONAL_B_SPLINE_SURFACE ( (
 ( 1.000000000000000000, 0.7071067811865482389, 1.000000000000000000),
 ( 1.000000000000000000, 0.7156795336770270799, 1.000000000000000000),
 ( 1.000000000000000000, 0.7224940905405163871, 1.000000000000000000),
 ( 1.000000000000000000, 0.7317806849512016321, 1.000000000000000000),
 ( 1.000000000000000000, 0.7342507314798352169, 1.000000000000000000),
 ( 1.000000000000000000, 0.7342566494600053506, 1.000000000000000000),
 ( 1.000000000000000000, 0.7244594855316945914, 1.000000000000000000),
 ( 1.000000000000000000, 0.7071067811865469066, 1.000000000000000000) ) ) 
 REPRESENTATION_ITEM ( '' )  SURFACE ( )  );
#3001 = CARTESIAN_POINT ( 'NONE',  ( -6.790153584124027475, 6.000000000000000000, -124.9643354754709748 ) ) ;
#3002 = DATE_AND_TIME ( #13673, #6157 ) ;
#3003 = CARTESIAN_POINT ( 'NONE',  ( -1.078957824791472619, 8.673617379884037444E-16, -133.0846919315902142 ) ) ;
#3004 = CARTESIAN_POINT ( 'NONE',  ( 1.052436484934203387, 2.075239479414269894, -1.000000000000007772 ) ) ;
#3005 = ORIENTED_EDGE ( 'NONE', *, *, #11838, .F. ) ;
#3006 = CARTESIAN_POINT ( 'NONE',  ( -67.58382170693636226, 10.00000000000000000, -204.5178482451963191 ) ) ;
#3007 = CARTESIAN_POINT ( 'NONE',  ( -3.249999999999999556, 3.750000000000000444, -3.500000000000000000 ) ) ;
#3008 = AXIS2_PLACEMENT_3D ( 'NONE', #13577, #5446, #9860 ) ;
#3009 = CARTESIAN_POINT ( 'NONE',  ( 2.298097038856278029, 9.125000000000000000, -5.798097038856279362 ) ) ;
#3010 = CARTESIAN_POINT ( 'NONE',  ( -2.397620167341370845, 9.999999999999998224, -107.6176329143618204 ) ) ;
#3011 = DIRECTION ( 'NONE',  ( 0.9982196940171963462, 0.000000000000000000, -0.05964429961207242531 ) ) ;
#3012 = CARTESIAN_POINT ( 'NONE',  ( 2.298097038856279362, 4.875000000000000000, -1.201902961143720860 ) ) ;
#3013 = CARTESIAN_POINT ( 'NONE',  ( -3.750000000000000000, 6.687500000000000888, -1.946699141100893149 ) ) ;
#3014 = ADVANCED_FACE ( 'NONE', ( #13787 ), #985, .T. ) ;
#3015 = CARTESIAN_POINT ( 'NONE',  ( -3.750000000000000000, 8.250000000000000000, -3.499999999999999112 ) ) ;
#3016 = DIRECTION ( 'NONE',  ( 0.8645818496218656835, 0.000000000000000000, -0.5024920151648518685 ) ) ;
#3017 = CARTESIAN_POINT ( 'NONE',  ( -7.749031843371119166, 1.142173573887167004, -116.8124745394366784 ) ) ;
#3018 = CARTESIAN_POINT ( 'NONE',  ( 1.553300858899109516, 9.437500000000000000, 0.2499999999999993616 ) ) ;
#3019 = DIRECTION ( 'NONE',  ( 0.000000000000000000, 1.000000000000000000, 0.000000000000000000 ) ) ;
#3020 = ORGANIZATION ( 'UNSPECIFIED', 'UNSPECIFIED', '' ) ;
#3021 = DIRECTION ( 'NONE',  ( 0.9961255586397049777, 0.000000000000000000, -0.08794243244723005948 ) ) ;
#3022 = CARTESIAN_POINT ( 'NONE',  ( 9.414574752465050267, 1.210099420865203834, -106.3373578080001209 ) ) ;
#3023 = CARTESIAN_POINT ( 'NONE',  ( -29.07636141981161515, 0.000000000000000000, -184.7664156487973912 ) ) ;
#3024 = CARTESIAN_POINT ( 'NONE',  ( 3.249999999999999112, 0.8125000000000001110, -2.153805922287439945 ) ) ;
#3025 = CARTESIAN_POINT ( 'NONE',  ( -31.41915002255961298, 15.00000000000000000, -151.2642837462047964 ) ) ;
#3026 = CARTESIAN_POINT ( 'NONE',  ( -3.249999999999999556, -0.2499999999999998890, -3.500000000000000000 ) ) ;
#3027 = ORIENTED_EDGE ( 'NONE', *, *, #916, .T. ) ;
#3028 = CYLINDRICAL_SURFACE ( 'NONE', #1060, 3.000000000000010214 ) ;
#3029 = CARTESIAN_POINT ( 'NONE',  ( 9.697553513687202198, 1.319436597465116101, -105.9306301742863496 ) ) ;
#3030 = CARTESIAN_POINT ( 'NONE',  ( -3.517695908037311803, 10.45879132743789341, -46.62865316603851085 ) ) ;
#3031 = LOCAL_TIME ( 12, 28, 20.00000000000000000, #4388 ) ;
#3032 = CARTESIAN_POINT ( 'NONE',  ( 1.346194077712558279, 7.062499999999999112, -6.750000000000000888 ) ) ;
#3033 = CARTESIAN_POINT ( 'NONE',  ( 27.13166404935670428, 5.000000000000000888, -138.0564292571840213 ) ) ;
#3034 = CARTESIAN_POINT ( 'NONE',  ( 3.750000000000000000, 12.75000000000000178, -3.500000000000000444 ) ) ;
#3035 = CIRCLE ( 'NONE', #1801, 1.000000000000042633 ) ;
#3036 = CARTESIAN_POINT ( 'NONE',  ( -62.99132485747528420, 15.00000000000000000, -202.4853500613857307 ) ) ;
#3037 = CARTESIAN_POINT ( 'NONE',  ( 0.000000000000000000, 0.000000000000000000, -0.5000000000000018874 ) ) ;
#3038 = CARTESIAN_POINT ( 'NONE',  ( -3.249999999999999556, 13.25000000000000000, -3.499999999999999556 ) ) ;
#3039 = CARTESIAN_POINT ( 'NONE',  ( 4.329912723285513465, 2.529993217055222399, -43.25836301743401435 ) ) ;
#3040 = CARTESIAN_POINT ( 'NONE',  ( -1.500000000000000000, 4.500000000000000888, 0.2500000000000002220 ) ) ;
#3041 = CARTESIAN_POINT ( 'NONE',  ( -1.346194077712559389, 7.437500000000000888, -6.749999999999999112 ) ) ;
#3042 = CARTESIAN_POINT ( 'NONE',  ( 6.363274845736492935, 5.000000000000000888, -132.2089327231056473 ) ) ;
#3043 = CARTESIAN_POINT ( 'NONE',  ( 10.95691125489327789, 11.77390254760747546, -44.42524603584411125 ) ) ;
#3044 = ORIENTED_EDGE ( 'NONE', *, *, #517, .F. ) ;
#3045 = CARTESIAN_POINT ( 'NONE',  ( 9.978323787696259828, 4.811580018084409716, -45.08809239636353539 ) ) ;
#3046 = CARTESIAN_POINT ( 'NONE',  ( -2.200833853042387211, 4.000000000000000000, -178.3042252324553942 ) ) ;
#3047 = CARTESIAN_POINT ( 'NONE',  ( 3.749999999999998668, 15.18750000000000355, -5.053300858899108405 ) ) ;
#3048 = AXIS2_PLACEMENT_3D ( 'NONE', #6073, #14206, #3453 ) ;
#3049 = CARTESIAN_POINT ( 'NONE',  ( -3.249999999999999112, 14.81250000000000355, -4.846194077712558723 ) ) ;
#3050 = CARTESIAN_POINT ( 'NONE',  ( 0.000000000000000000, 13.50000000000000178, -0.2500000000000002220 ) ) ;
#3051 = ORIENTED_EDGE ( 'NONE', *, *, #9325, .F. ) ;
#3052 = CARTESIAN_POINT ( 'NONE',  ( 2.298097038856278473, 11.62500000000000000, -5.798097038856279362 ) ) ;
#3053 = CARTESIAN_POINT ( 'NONE',  ( 10.97120741197404570, 11.75624598098227303, -44.98549899094406612 ) ) ;
#3054 = CARTESIAN_POINT ( 'NONE',  ( 10.00369055844187649, 12.49999999999999822, -46.08764602067113714 ) ) ;
#3055 = CARTESIAN_POINT ( 'NONE',  ( 4.945012662353664545, 1.189081421482657053, 3.158926035384847175 ) ) ;
#3056 = CARTESIAN_POINT ( 'NONE',  ( -6.510167201456665609, 14.56253871824070956, -117.0692195733290504 ) ) ;
#3057 = CALENDAR_DATE ( 2026, 8, 10 ) ;
#3058 = AXIS2_PLACEMENT_3D ( 'NONE', #12363, #3019, #7645 ) ;
#3059 = CARTESIAN_POINT ( 'NONE',  ( 8.541738004265454265, 12.49999999999999822, -116.2437985783182057 ) ) ;
#3060 = CARTESIAN_POINT ( 'NONE',  ( 20.87131526946576443, 1.301042606982605321E-15, -138.9752963459259547 ) ) ;
#3061 = EDGE_LOOP ( 'NONE', ( #6055, #8446, #1976, #14980 ) ) ;
#3062 = EDGE_CURVE ( 'NONE', #2133, #2207, #12988, .T. ) ;
#3063 = CARTESIAN_POINT ( 'NONE',  ( 3.249999999999998668, 4.687500000000000888, -4.846194077712560500 ) ) ;
#3064 = CARTESIAN_POINT ( 'NONE',  ( 4.286263797015736595E-16, 4.000000000000000000, 3.500000000000000000 ) ) ;
#3065 = CARTESIAN_POINT ( 'NONE',  ( 3.749999999999999556, 3.250000000000000000, -3.500000000000000444 ) ) ;
#3066 = ORIENTED_EDGE ( 'NONE', *, *, #13094, .F. ) ;
#3067 = CARTESIAN_POINT ( 'NONE',  ( 26.22222779830891781, 1.750000000000000000, 70.75745246403606359 ) ) ;
#3068 = CARTESIAN_POINT ( 'NONE',  ( -3.750000000000000000, 0.2500000000000000555, -3.499999999999999112 ) ) ;
#3069 = CARTESIAN_POINT ( 'NONE',  ( 7.262177415846634787, 3.361685231369096805, -24.56097010744011300 ) ) ;
#3070 = CARTESIAN_POINT ( 'NONE',  ( 0.06817676530921484845, -0.03742728397158888443, 0.7722394814505989524 ) ) ;
#3071 = CARTESIAN_POINT ( 'NONE',  ( -1.553300858899107073, 0.4375000000000000555, -7.250000000000000000 ) ) ;
#3072 = DATE_AND_TIME ( #6629, #1795 ) ;
#3073 = CARTESIAN_POINT ( 'NONE',  ( -3.648797883638982054, 2.490287375297123962, -1.000000000000000888 ) ) ;
#3074 = AXIS2_PLACEMENT_3D ( 'NONE', #12181, #1746, #14521 ) ;
#3075 = DIRECTION ( 'NONE',  ( 0.000000000000000000, 0.000000000000000000, -1.000000000000000000 ) ) ;
#3076 = ORIENTED_EDGE ( 'NONE', *, *, #11316, .T. ) ;
#3077 = EDGE_CURVE ( 'NONE', #10989, #11588, #8048, .T. ) ;
#3078 = CARTESIAN_POINT ( 'NONE',  ( -30.41959608467592702, 15.00000000000000355, -151.3633174574383418 ) ) ;
#3079 = CARTESIAN_POINT ( 'NONE',  ( 3.249999999999998224, 3.187500000000000444, -4.846194077712561388 ) ) ;
#3080 = DIRECTION ( 'NONE',  ( 0.02181900108494663065, 0.000000000000000000, -0.9997619372588932851 ) ) ;
#3081 = DIRECTION ( 'NONE',  ( 0.000000000000000000, 0.000000000000000000, -1.000000000000000000 ) ) ;
#3082 = CARTESIAN_POINT ( 'NONE',  ( -4.592425496802573972E-16, 7.000000000000000000, -7.250000000000000000 ) ) ;
#3083 = CARTESIAN_POINT ( 'NONE',  ( 3.750000000000000000, 7.750000000000000000, -3.500000000000000444 ) ) ;
#3084 = CARTESIAN_POINT ( 'NONE',  ( -2.869987474717050624, 2.075239479414269894, -1.000000000000000888 ) ) ;
#3085 = CARTESIAN_POINT ( 'NONE',  ( 1.500000000000000000, 4.500000000000000888, 0.2500000000000002220 ) ) ;
#3086 = CARTESIAN_POINT ( 'NONE',  ( 3.749999999999999112, 9.187500000000001776, -5.053300858899108405 ) ) ;
#3087 = DIRECTION ( 'NONE',  ( -0.1564344650402312298, -0.000000000000000000, 0.9876883405951376593 ) ) ;
#3088 = CC_DESIGN_PERSON_AND_ORGANIZATION_ASSIGNMENT ( #1900, #13800, ( #2439 ) ) ;
#3089 = CARTESIAN_POINT ( 'NONE',  ( -9.306320601523863090, -2.743867526398026335, -40.23124431751399044 ) ) ;
#3090 = CARTESIAN_POINT ( 'NONE',  ( 9.531305032586972814, 1.319851304386060020, -106.3909117981410901 ) ) ;
#3091 = EDGE_LOOP ( 'NONE', ( #11307, #6248, #1248, #4284 ) ) ;
#3092 = ADVANCED_FACE ( 'NONE', ( #12776 ), #12621, .T. ) ;
#3093 = CARTESIAN_POINT ( 'NONE',  ( -29.84187669631901940, -8.150263268976921852E-13, -194.0986676374979822 ) ) ;
#3094 = DIRECTION ( 'NONE',  ( -0.9961255586397050887, 0.000000000000000000, 0.08794243244723005948 ) ) ;
#3095 = ADVANCED_FACE ( 'NONE', ( #2183 ), #9139, .F. ) ;
#3096 = FACE_OUTER_BOUND ( 'NONE', #9098, .T. ) ;
#3097 = EDGE_CURVE ( 'NONE', #4358, #11999, #6887, .T. ) ;
#3098 = CARTESIAN_POINT ( 'NONE',  ( 3.249999999999998224, 2.187500000000000000, -4.846194077712561388 ) ) ;
#3099 = ORIENTED_EDGE ( 'NONE', *, *, #12258, .T. ) ;
#3100 = CARTESIAN_POINT ( 'NONE',  ( -11.40820045174505992, 9.999999999999998224, -126.3212311505415784 ) ) ;
#3101 = DIRECTION ( 'NONE',  ( 0.000000000000000000, 0.000000000000000000, -1.000000000000000000 ) ) ;
#3102 = DIRECTION ( 'NONE',  ( 0.000000000000000000, -1.000000000000000000, 0.000000000000000000 ) ) ;
#3103 = CARTESIAN_POINT ( 'NONE',  ( -1.346194077712559389, 10.06250000000000000, -0.2500000000000002220 ) ) ;
#3104 = FACE_OUTER_BOUND ( 'NONE', #7924, .T. ) ;
#3105 = CARTESIAN_POINT ( 'NONE',  ( -6.992168204694889866, 8.673617379884035472E-16, -113.2636094677359893 ) ) ;
#3106 = CARTESIAN_POINT ( 'NONE',  ( -3.249999999999999112, 9.687500000000000000, -2.153805922287440833 ) ) ;
#3107 = CARTESIAN_POINT ( 'NONE',  ( 51.19063959271458231, 0.000000000000000000, 70.62932606827693860 ) ) ;
#3108 = CARTESIAN_POINT ( 'NONE',  ( 1.553300858899105963, 12.56250000000000000, -7.250000000000000888 ) ) ;
#3109 = CARTESIAN_POINT ( 'NONE',  ( -68.68211634358988249, 15.00000000000000000, -201.9941738958162603 ) ) ;
#3110 = CARTESIAN_POINT ( 'NONE',  ( -4.403991534456141999, 15.00000000000000178, -103.3272078610332301 ) ) ;
#3111 = CARTESIAN_POINT ( 'NONE',  ( -3.249999999999999556, 13.18749999999999822, -2.153805922287440833 ) ) ;
#3112 = DIRECTION ( 'NONE',  ( 1.000000000000000000, 0.000000000000000000, 0.000000000000000000 ) ) ;
#3113 = CARTESIAN_POINT ( 'NONE',  ( -8.289881740238502772, -2.075239479414269894, -35.21986562831451550 ) ) ;
#3114 = CARTESIAN_POINT ( 'NONE',  ( -3.980102097228897245E-16, 8.500000000000000000, -6.749999999999999112 ) ) ;
#3115 = CARTESIAN_POINT ( 'NONE',  ( 3.201254193339545751, 3.381110835560071859, 4.950899197493613180 ) ) ;
#3116 = CARTESIAN_POINT ( 'NONE',  ( -12.27209645382209402, 2.500000000000000444, -127.2227734861304782 ) ) ;
#3117 = VERTEX_POINT ( 'NONE', #15188 ) ;
#3118 = CYLINDRICAL_SURFACE ( 'NONE', #9552, 2.326940983401415419 ) ;
#3119 = CARTESIAN_POINT ( 'NONE',  ( 9.032890029152659039, 12.50000000000000355, -118.1323615500725310 ) ) ;
#3120 = CARTESIAN_POINT ( 'NONE',  ( -3.749999999999999556, 0.3125000000000000555, -5.053300858899104853 ) ) ;
#3121 = CARTESIAN_POINT ( 'NONE',  ( -3.750000000000000000, 1.687499999999999778, -1.946699141100893149 ) ) ;
#3122 = CARTESIAN_POINT ( 'NONE',  ( -2.298097038856279362, 13.87500000000000178, -5.798097038856278473 ) ) ;
#3123 = ORIENTED_EDGE ( 'NONE', *, *, #801, .F. ) ;
#3124 = CARTESIAN_POINT ( 'NONE',  ( 1.346194077712558057, 11.56249999999999822, -6.750000000000000000 ) ) ;
#3125 = DIRECTION ( 'NONE',  ( -0.1564344650402312298, -0.000000000000000000, 0.9876883405951376593 ) ) ;
#3126 = B_SPLINE_CURVE_WITH_KNOTS ( 'NONE', 3,
 ( #14708, #12361, #10269, #13830, #5332, #3233, #10046, #7867, #10119, #14860 ),
 .UNSPECIFIED., .F., .F.,
 ( 4, 2, 2, 2, 4 ),
 ( 0.000000000000000000, 0.01436113971778546841, 0.02872227943557093682, 0.04308341915335640870, 0.05744455887114187365 ),
 .UNSPECIFIED. ) ;
#3127 = CARTESIAN_POINT ( 'NONE',  ( -9.055672782877035587, 11.36792136377893492, -104.6047652700399198 ) ) ;
#3128 = CARTESIAN_POINT ( 'NONE',  ( 5.238157166760104566, 1.649858934233373597, 3.774848331988833738 ) ) ;
#3129 = CARTESIAN_POINT ( 'NONE',  ( -8.455319114079282272, 13.21761715718190899, -116.6570696633502706 ) ) ;
#3130 = CARTESIAN_POINT ( 'NONE',  ( 5.856043916822682327, 15.00000000000000000, -115.1238147290586653 ) ) ;
#3131 = CARTESIAN_POINT ( 'NONE',  ( 0.2499999999999999445, 5.000000000000000000, 0.2500000000000002220 ) ) ;
#3132 = CARTESIAN_POINT ( 'NONE',  ( 25.22814042709519100, 1.659276419493565857, -137.4257722450890356 ) ) ;
#3133 = ORIENTED_EDGE ( 'NONE', *, *, #981, .F. ) ;
#3134 = CARTESIAN_POINT ( 'NONE',  ( -1.346194077712559389, 4.062500000000000000, -0.2500000000000002220 ) ) ;
#3135 = CYLINDRICAL_SURFACE ( 'NONE', #7983, 2.500000000000000000 ) ;
#3136 = CARTESIAN_POINT ( 'NONE',  ( 3.750000000000000000, 3.312500000000000000, -1.946699141100892705 ) ) ;
#3137 = EDGE_LOOP ( 'NONE', ( #12523, #12066, #11392, #5379 ) ) ;
#3138 = DIRECTION ( 'NONE',  ( -0.9997619372588932851, 0.000000000000000000, -0.02181900108494672086 ) ) ;
#3139 = CARTESIAN_POINT ( 'NONE',  ( 0.000000000000000000, 6.000000000000000000, 0.2500000000000002220 ) ) ;
#3140 = CARTESIAN_POINT ( 'NONE',  ( 9.940211158120405344, 12.49999999999999822, -43.17897536272747772 ) ) ;
#3141 = CARTESIAN_POINT ( 'NONE',  ( -4.234402844927150689, 0.000000000000000000, -117.4888040839639558 ) ) ;
#3142 = CARTESIAN_POINT ( 'NONE',  ( 1.553300858899108849, 2.937500000000000000, 0.2499999999999993616 ) ) ;
#3143 = MECHANICAL_CONTEXT ( 'NONE', #6610, 'mechanical' ) ;
#3144 = CARTESIAN_POINT ( 'NONE',  ( 10.50985052422430321, 5.000000000000000888, -107.7177067850638679 ) ) ;
#3145 = DIRECTION ( 'NONE',  ( 0.02181900108494707474, 0.000000000000000000, -0.9997619372588931741 ) ) ;
#3146 = ORIENTED_EDGE ( 'NONE', *, *, #4363, .T. ) ;
#3147 = CARTESIAN_POINT ( 'NONE',  ( 2.298097038856279362, 2.375000000000000000, -1.201902961143720860 ) ) ;
#3148 = LINE ( 'NONE', #6634, #10443 ) ;
#3149 = CARTESIAN_POINT ( 'NONE',  ( -8.645680077725348411, 2.500000000000000444, -122.8677831016847790 ) ) ;
#3150 = CARTESIAN_POINT ( 'NONE',  ( -1.553300858899107073, 8.937500000000000000, -7.249999999999999112 ) ) ;
#3151 = CARTESIAN_POINT ( 'NONE',  ( 0.000000000000000000, 12.00000000000000000, 0.2500000000000002220 ) ) ;
#3152 = EDGE_CURVE ( 'NONE', #9480, #333, #248, .T. ) ;
#3153 = DIRECTION ( 'NONE',  ( 0.000000000000000000, 0.9314983497198057183, 0.3637455490714332496 ) ) ;
#3154 = CARTESIAN_POINT ( 'NONE',  ( -8.506498296742686094, 1.839370509249187213, -116.6455419169649446 ) ) ;
#3155 = CARTESIAN_POINT ( 'NONE',  ( -1.346194077712559389, 8.437500000000000000, -6.749999999999999112 ) ) ;
#3156 = CARTESIAN_POINT ( 'NONE',  ( -3.749999999999999556, 9.750000000000000000, -3.499999999999999112 ) ) ;
#3157 = CARTESIAN_POINT ( 'NONE',  ( 4.999961392659725057, -8.122774307663799537E-14, -31.10603894082280263 ) ) ;
#3158 = CARTESIAN_POINT ( 'NONE',  ( 5.783145697618031100, 15.00000000000000178, -114.0858433367058637 ) ) ;
#3159 = CYLINDRICAL_SURFACE ( 'NONE', #8153, 0.4999999999999726885 ) ;
#3160 = ORIENTED_EDGE ( 'NONE', *, *, #12337, .F. ) ;
#3161 = CARTESIAN_POINT ( 'NONE',  ( -25.32823296183972417, 0.000000000000000000, -187.0457223361869410 ) ) ;
#3162 = CARTESIAN_POINT ( 'NONE',  ( 12.72476843650552425, 3.715092006986288720, -166.5695719882495496 ) ) ;
#3163 = CARTESIAN_POINT ( 'NONE',  ( -54.08656694241062013, 15.00000000000000000, -162.1624640010098517 ) ) ;
#3164 = CARTESIAN_POINT ( 'NONE',  ( -3.249999999999999556, 2.750000000000000444, -3.500000000000000000 ) ) ;
#3165 = EDGE_LOOP ( 'NONE', ( #10848, #10915, #4081, #1381 ) ) ;
#3166 = CARTESIAN_POINT ( 'NONE',  ( 9.939878312292620421, 9.999999999999998224, -115.2320631035898373 ) ) ;
#3167 = CARTESIAN_POINT ( 'NONE',  ( 9.186974873226770200, 0.9102337534740122527, -105.7859147073006767 ) ) ;
#3168 =( BOUNDED_SURFACE ( )  B_SPLINE_SURFACE ( 3, 1, ( 
 ( #9018, #10027 ),
 ( #6466, #9873 ),
 ( #6547, #8942 ),
 ( #6626, #4009 ) ),
 .UNSPECIFIED., .F., .F., .T. ) 
 B_SPLINE_SURFACE_WITH_KNOTS ( ( 4, 4 ),
 ( 2, 2 ),
 ( 0.000000000000000000, 1.000000000000000000 ),
 ( 0.000000000000000000, 1.000000000000000000 ),
 .UNSPECIFIED. ) 
 GEOMETRIC_REPRESENTATION_ITEM ( )  RATIONAL_B_SPLINE_SURFACE ( (
 ( 1.000000000000000000, 1.000000000000000000),
 ( 0.8388501503673406745, 0.8388501503673406745),
 ( 0.8388501503673406745, 0.8388501503673406745),
 ( 1.000000000000000000, 1.000000000000000000) ) ) 
 REPRESENTATION_ITEM ( '' )  SURFACE ( )  );
#3169 = CARTESIAN_POINT ( 'NONE',  ( -1.843872751574030300, 15.00000000000000000, -133.9216539038831399 ) ) ;
#3170 = CARTESIAN_POINT ( 'NONE',  ( 8.875022500030622652, 10.34680280068111458, 5.628716254818995957 ) ) ;
#3171 = CARTESIAN_POINT ( 'NONE',  ( -0.5126277339614576656, -3.286289637815826199E-12, -103.6859198938546882 ) ) ;
#3172 = CARTESIAN_POINT ( 'NONE',  ( 3.249999999999998224, 10.18750000000000533, -4.846194077712561388 ) ) ;
#3173 = EDGE_CURVE ( 'NONE', #2695, #9540, #5777, .T. ) ;
#3174 = DIRECTION ( 'NONE',  ( 1.000000000000000000, 0.000000000000000000, 0.000000000000000000 ) ) ;
#3175 = CARTESIAN_POINT ( 'NONE',  ( -4.592425496802573972E-16, 14.50000000000000000, -7.249999999999999112 ) ) ;
#3176 = PERSON ( 'UNSPECIFIED', 'UNSPECIFIED', 'UNSPECIFIED', ('UNSPECIFIED'), ('UNSPECIFIED'), ('UNSPECIFIED') ) ;
#3177 = CARTESIAN_POINT ( 'NONE',  ( -69.06832266532519782, 9.999999999999998224, -200.7467498273179274 ) ) ;
#3178 = ADVANCED_FACE ( 'NONE', ( #14313 ), #14401, .F. ) ;
#3179 = CARTESIAN_POINT ( 'NONE',  ( 1.668807522230304041, 2.569799602646715808, -1.000000000000001110 ) ) ;
#3180 = CARTESIAN_POINT ( 'NONE',  ( 1.346194077712560944, 10.93750000000000000, -0.2500000000000010547 ) ) ;
#3181 = CARTESIAN_POINT ( 'NONE',  ( -8.105036670657762343, 10.00000000000000178, -106.2142721819313920 ) ) ;
#3182 = CARTESIAN_POINT ( 'NONE',  ( 4.548248957081511001, 14.25778345964358529, 2.149752393844249543 ) ) ;
#3183 = CARTESIAN_POINT ( 'NONE',  ( -3.980102097228897245E-16, 10.50000000000000000, -6.749999999999999112 ) ) ;
#3184 = CARTESIAN_POINT ( 'NONE',  ( 10.01939027896081313, 5.000000000000000888, -127.6977514918621637 ) ) ;
#3185 = FACE_OUTER_BOUND ( 'NONE', #6854, .T. ) ;
#3186 = ORIENTED_EDGE ( 'NONE', *, *, #2525, .T. ) ;
#3187 = ORIENTED_EDGE ( 'NONE', *, *, #979, .T. ) ;
#3188 = CARTESIAN_POINT ( 'NONE',  ( -10.42889815920712060, 4.000000000000000000, -186.8962127970309837 ) ) ;
#3189 = CARTESIAN_POINT ( 'NONE',  ( 2.651650429449552870, 1.625000000000000222, -6.151650429449554203 ) ) ;
#3190 = CARTESIAN_POINT ( 'NONE',  ( 2.651650429449552870, 2.125000000000000000, -6.151650429449553314 ) ) ;
#3191 = CARTESIAN_POINT ( 'NONE',  ( -3.249999999999999556, 13.75000000000000000, -3.500000000000000000 ) ) ;
#3192 = ORIENTED_EDGE ( 'NONE', *, *, #9515, .T. ) ;
#3193 = CARTESIAN_POINT ( 'NONE',  ( 3.249999999999999556, 11.75000000000000000, -3.500000000000000000 ) ) ;
#3194 = CARTESIAN_POINT ( 'NONE',  ( 10.02828843047459095, 11.77391908303435208, -44.24972543469815633 ) ) ;
#3195 = EDGE_CURVE ( 'NONE', #5598, #14191, #2220, .T. ) ;
#3196 = CC_DESIGN_APPROVAL ( #2928, ( #13819 ) ) ;
#3197 = CARTESIAN_POINT ( 'NONE',  ( -9.240119717576694924, 9.999999999999998224, -104.6630069175297564 ) ) ;
#3198 = CARTESIAN_POINT ( 'NONE',  ( -7.230043083586023656, 14.09412780563432221, -116.2995594653081355 ) ) ;
#3199 = CIRCLE ( 'NONE', #5186, 3.500000000000003109 ) ;
#3200 = PERSON_AND_ORGANIZATION ( #3176, #3020 ) ;
#3201 = CARTESIAN_POINT ( 'NONE',  ( 5.834340755081701246, 15.00000000000000000, -112.9803539749909902 ) ) ;
#3202 = DIRECTION ( 'NONE',  ( 0.000000000000000000, 1.000000000000000000, 0.000000000000000000 ) ) ;
#3203 = ORIENTED_EDGE ( 'NONE', *, *, #13851, .T. ) ;
#3204 = CARTESIAN_POINT ( 'NONE',  ( 23.63626030785080090, 0.5263503646225780042, -138.6462866365781963 ) ) ;
#3205 = CARTESIAN_POINT ( 'NONE',  ( -3.249999999999999556, 11.31249999999999822, -4.846194077712557835 ) ) ;
#3206 = ORIENTED_EDGE ( 'NONE', *, *, #1022, .T. ) ;
#3207 = CARTESIAN_POINT ( 'NONE',  ( 2.298097038856279362, 5.875000000000000000, -1.201902961143720860 ) ) ;
#3208 = CARTESIAN_POINT ( 'NONE',  ( -9.030574454602195544, -2.490287375297124406, -34.97919997656152447 ) ) ;
#3209 = CARTESIAN_POINT ( 'NONE',  ( -3.750000000000000000, 1.812499999999999778, -5.053300858899105741 ) ) ;
#3210 = ORIENTED_EDGE ( 'NONE', *, *, #8656, .F. ) ;
#3211 = DIRECTION ( 'NONE',  ( -0.000000000000000000, -1.000000000000000000, -0.000000000000000000 ) ) ;
#3212 = CARTESIAN_POINT ( 'NONE',  ( 1.346194077712558057, 0.5625000000000001110, -6.750000000000000000 ) ) ;
#3213 = VECTOR ( 'NONE', #1262, 1000.000000000000000 ) ;
#3214 = CARTESIAN_POINT ( 'NONE',  ( 0.000000000000000000, 5.000000000000000000, 0.2500000000000002220 ) ) ;
#3215 = CARTESIAN_POINT ( 'NONE',  ( -24.92455668927321000, 1.982032305341395295, -207.3388352837438049 ) ) ;
#3216 = CARTESIAN_POINT ( 'NONE',  ( 0.2328350733780833737, -8.673617379884037444E-16, -127.8934642279842819 ) ) ;
#3217 = COORDINATED_UNIVERSAL_TIME_OFFSET ( 0, 0, .AHEAD. ) ;
#3218 = AXIS2_PLACEMENT_3D ( 'NONE', #4135, #12388, #13863 ) ;
#3219 = CARTESIAN_POINT ( 'NONE',  ( 12.10928247722332074, 5.000000000000000000, -123.8687610530459438 ) ) ;
#3220 = VECTOR ( 'NONE', #5191, 1000.000000000000000 ) ;
#3221 = LINE ( 'NONE', #13907, #15096 ) ;
#3222 = CIRCLE ( 'NONE', #5923, 6.000000000000002665 ) ;
#3223 = AXIS2_PLACEMENT_3D ( 'NONE', #8482, #11878, #9563 ) ;
#3224 = VERTEX_POINT ( 'NONE', #1101 ) ;
#3225 = CARTESIAN_POINT ( 'NONE',  ( 0.000000000000000000, 4.499999999999999112, -0.2500000000000002220 ) ) ;
#3226 = DIRECTION ( 'NONE',  ( 0.000000000000000000, -1.000000000000000000, 0.000000000000000000 ) ) ;
#3227 = VECTOR ( 'NONE', #10584, 1000.000000000000000 ) ;
#3228 = VECTOR ( 'NONE', #266, 1000.000000000000227 ) ;
#3229 = CARTESIAN_POINT ( 'NONE',  ( 1.553300858899105963, 8.062500000000001776, -7.249999999999999112 ) ) ;
#3230 = CARTESIAN_POINT ( 'NONE',  ( -3.750000000000000000, 14.18750000000000000, -1.946699141100892927 ) ) ;
#3231 = CARTESIAN_POINT ( 'NONE',  ( 6.369258321017759350, 2.075239479414269894, -34.56909192082981974 ) ) ;
#3232 = ORIENTED_EDGE ( 'NONE', *, *, #140, .F. ) ;
#3233 = CARTESIAN_POINT ( 'NONE',  ( 11.91826453496364380, -2.051692149507289097E-14, 18.75693026131821028 ) ) ;
#3234 = CARTESIAN_POINT ( 'NONE',  ( 3.249999999999998224, 1.187500000000000222, -4.846194077712561388 ) ) ;
#3235 = CARTESIAN_POINT ( 'NONE',  ( -4.125453648579471277, 4.336808689942017736E-16, -107.3641501471127526 ) ) ;
#3236 = DIRECTION ( 'NONE',  ( -0.7437943690223837168, 0.000000000000000000, -0.6684085102769072861 ) ) ;
#3237 = DIRECTION ( 'NONE',  ( 0.05964429961207245307, 0.000000000000000000, 0.9982196940171964572 ) ) ;
#3238 =( GEOMETRIC_REPRESENTATION_CONTEXT ( 3 ) GLOBAL_UNCERTAINTY_ASSIGNED_CONTEXT ( ( #4788 ) ) GLOBAL_UNIT_ASSIGNED_CONTEXT ( ( #12712, #9372, #2124 ) ) REPRESENTATION_CONTEXT ( 'NONE', 'WORKASPACE' ) );
#3239 = ORIENTED_EDGE ( 'NONE', *, *, #4488, .F. ) ;
#3240 = CARTESIAN_POINT ( 'NONE',  ( -28.09207221025136292, 4.000000000000024869, -205.1456435447945807 ) ) ;
#3241 = CARTESIAN_POINT ( 'NONE',  ( 6.369258321017760238, -2.529993217055220178, -34.56909192082981974 ) ) ;
#3242 = CARTESIAN_POINT ( 'NONE',  ( -43.80089141906720585, 15.00000000000000000, -153.5888841403339597 ) ) ;
#3243 = ADVANCED_FACE ( 'NONE', ( #1327 ), #10359, .F. ) ;
#3244 = CARTESIAN_POINT ( 'NONE',  ( -1.346194077712558945, 1.562500000000000222, -0.2500000000000002220 ) ) ;
#3245 = VERTEX_POINT ( 'NONE', #8423 ) ;
#3246 = CARTESIAN_POINT ( 'NONE',  ( -12.27209645382210113, 9.999999999999998224, -127.2227734861304782 ) ) ;
#3247 = DIRECTION ( 'NONE',  ( 0.003262051938530752433, 0.000000000000000000, 0.9999946794944213346 ) ) ;
#3248 = DIRECTION ( 'NONE',  ( 0.002879925520664897674, 0.000000000000000000, 0.9999958530058988826 ) ) ;
#3249 = CARTESIAN_POINT ( 'NONE',  ( 8.962104331735417873, 14.96030145802490097, 1.638565632197652944 ) ) ;
#3250 = CARTESIAN_POINT ( 'NONE',  ( -1.499260709785477097, 5.000000000000000888, -106.0110764665418515 ) ) ;
#3251 = CARTESIAN_POINT ( 'NONE',  ( 0.000000000000000000, 10.50000000000000000, -0.2500000000000002220 ) ) ;
#3252 = TOROIDAL_SURFACE ( 'NONE', #13388, 2.000000000000009326, 1.000000000000000000 ) ;
#3253 = DIRECTION ( 'NONE',  ( 0.000000000000000000, -1.000000000000000000, 0.000000000000000000 ) ) ;
#3254 = CARTESIAN_POINT ( 'NONE',  ( 2.651650429449552870, 4.125000000000000000, -6.151650429449555091 ) ) ;
#3255 = CARTESIAN_POINT ( 'NONE',  ( 0.000000000000000000, 1.000000000000000000, 0.000000000000000000 ) ) ;
#3256 = CARTESIAN_POINT ( 'NONE',  ( -8.375425654315606039, 12.27215496146240703, -105.2394517302402619 ) ) ;
#3257 = CARTESIAN_POINT ( 'NONE',  ( -3.249999999999999556, 14.25000000000000000, -3.499999999999999556 ) ) ;
#3258 = DIRECTION ( 'NONE',  ( 0.000000000000000000, 1.000000000000000000, 0.000000000000000000 ) ) ;
#3259 = CARTESIAN_POINT ( 'NONE',  ( -8.289881740238502772, -2.075239479414269894, -35.21986562831451550 ) ) ;
#3260 = CARTESIAN_POINT ( 'NONE',  ( -3.249999999999999556, 8.250000000000000000, -3.499999999999999556 ) ) ;
#3261 = CARTESIAN_POINT ( 'NONE',  ( 3.000122744334918767, 1.017992234156722242, 3.255451705640021842 ) ) ;
#3262 = CARTESIAN_POINT ( 'NONE',  ( 1.320501113854931630, 10.00000000000000000, -137.8664870916819893 ) ) ;
#3263 = LOCAL_TIME ( 12, 28, 20.00000000000000000, #8174 ) ;
#3264 = ORIENTED_EDGE ( 'NONE', *, *, #13113, .F. ) ;
#3265 = ADVANCED_FACE ( 'NONE', ( #6030 ), #13157, .T. ) ;
#3266 = ORIENTED_EDGE ( 'NONE', *, *, #6474, .T. ) ;
#3267 = CARTESIAN_POINT ( 'NONE',  ( -18.37680385559763963, 3.999999999999999112, -197.3497678893306215 ) ) ;
#3268 = CARTESIAN_POINT ( 'NONE',  ( 1.553300858899105963, 1.562500000000000000, -7.250000000000000888 ) ) ;
#3269 = CARTESIAN_POINT ( 'NONE',  ( 2.298097038856278029, 15.12500000000000000, -5.798097038856279362 ) ) ;
#3270 = ADVANCED_FACE ( 'NONE', ( #3492 ), #12055, .T. ) ;
#3271 = CARTESIAN_POINT ( 'NONE',  ( -0.3766621274091715987, -0.2500000000000000000, -0.1347136637304948981 ) ) ;
#3272 = ORIENTED_EDGE ( 'NONE', *, *, #916, .F. ) ;
#3273 = CARTESIAN_POINT ( 'NONE',  ( -2.298097038856278473, 13.12500000000000000, -1.201902961143720416 ) ) ;
#3274 = CARTESIAN_POINT ( 'NONE',  ( -2.987113812559607062, -2.409215066305300912, -1.000000000000001332 ) ) ;
#3275 = CARTESIAN_POINT ( 'NONE',  ( -9.201659748534703809, 10.69856349024409425, -104.6507959483510604 ) ) ;
#3276 = CARTESIAN_POINT ( 'NONE',  ( 1.346194077712558057, 2.562500000000000444, -6.750000000000000000 ) ) ;
#3277 = PERSON_AND_ORGANIZATION ( #14996, #2470 ) ;
#3278 = APPROVAL ( #14754, 'UNKNOWN' ) ;
#3279 = CARTESIAN_POINT ( 'NONE',  ( 5.818533358179984738, 15.00000000000000000, -114.5878108573819247 ) ) ;
#3280 = DIRECTION ( 'NONE',  ( 0.000000000000000000, 1.000000000000000000, 0.000000000000000000 ) ) ;
#3281 = VERTEX_POINT ( 'NONE', #9754 ) ;
#3282 = AXIS2_PLACEMENT_3D ( 'NONE', #9719, #14452, #8546 ) ;
#3283 = CARTESIAN_POINT ( 'NONE',  ( 26.30091364428284351, 3.130032034343683378, -137.0310972895143209 ) ) ;
#3284 = CARTESIAN_POINT ( 'NONE',  ( -1.346194077712558945, 12.06250000000000000, -0.2500000000000002220 ) ) ;
#3285 = ORIENTED_EDGE ( 'NONE', *, *, #12925, .F. ) ;
#3286 = EDGE_CURVE ( 'NONE', #4560, #2776, #2290, .T. ) ;
#3287 = ORIENTED_EDGE ( 'NONE', *, *, #8631, .F. ) ;
#3288 = CARTESIAN_POINT ( 'NONE',  ( 0.000000000000000000, 3.000000000000000000, -0.2500000000000002220 ) ) ;
#3289 = DIRECTION ( 'NONE',  ( 0.000000000000000000, -1.000000000000000000, 0.000000000000000000 ) ) ;
#3290 = CARTESIAN_POINT ( 'NONE',  ( -4.592425496802573972E-16, 3.000000000000000444, -7.250000000000000000 ) ) ;
#3291 = EDGE_CURVE ( 'NONE', #11406, #7450, #3880, .T. ) ;
#3292 = CARTESIAN_POINT ( 'NONE',  ( -2.298097038856278029, 5.625000000000000888, -1.201902961143720638 ) ) ;
#3294 = ADVANCED_FACE ( 'NONE', ( #5748 ), #1042, .T. ) ;
#3293 = ORIENTED_EDGE ( 'NONE', *, *, #14235, .F. ) ;
#3295 = B_SPLINE_CURVE_WITH_KNOTS ( 'NONE', 3,
 ( #12252, #12009, #1435, #714, #5418, #13705, #4271, #7815, #6141, #275, #4990, #3834, #2248, #5640, #11592, #1159 ),
 .UNSPECIFIED., .F., .F.,
 ( 4, 2, 2, 2, 2, 2, 2, 4 ),
 ( 3.469446951953614189E-18, 0.006235229064615841442, 0.01247045812923167941, 0.01870568719384751652, 0.02182330172615543767, 0.02494091625846335536, 0.03741137438769520651, 0.04988183251692705766 ),
 .UNSPECIFIED. ) ;
#3296 = CARTESIAN_POINT ( 'NONE',  ( -1.528156170053301510, 7.379999999999995453, -45.73714083922575213 ) ) ;
#3297 = CARTESIAN_POINT ( 'NONE',  ( -1.346194077712559389, 0.06250000000000000000, -0.2500000000000002220 ) ) ;
#3298 = CARTESIAN_POINT ( 'NONE',  ( -1.553300858899106629, 4.062500000000000000, 0.2500000000000002220 ) ) ;
#3299 = CIRCLE ( 'NONE', #1825, 1.000000000000000000 ) ;
#3300 = AXIS2_PLACEMENT_3D ( 'NONE', #15057, #10250, #2988 ) ;
#3301 = CARTESIAN_POINT ( 'NONE',  ( -24.82503501351391151, 2.452721149805614953, -207.8977114406789326 ) ) ;
#3302 = DIRECTION ( 'NONE',  ( 1.000000000000000000, 0.000000000000000000, 0.000000000000000000 ) ) ;
#3303 = PERSON_AND_ORGANIZATION_ROLE ( 'classification_officer' ) ;
#3304 = CARTESIAN_POINT ( 'NONE',  ( 10.81974369748103371, 5.000000000000000000, -121.8879343890986888 ) ) ;
#3305 = ORIENTED_EDGE ( 'NONE', *, *, #4143, .T. ) ;
#3306 = VECTOR ( 'NONE', #13533, 1000.000000000000227 ) ;
#3307 = CARTESIAN_POINT ( 'NONE',  ( 1.346194077712561166, 5.437500000000000888, -0.2500000000000011102 ) ) ;
#3308 = CARTESIAN_POINT ( 'NONE',  ( 4.248871783098677746, 15.00000000000000000, -126.1456066832004126 ) ) ;
#3309 = PRODUCT_RELATED_PRODUCT_CATEGORY ( 'detail', '', ( #6227 ) ) ;
#3310 = CARTESIAN_POINT ( 'NONE',  ( -4.592425496802573972E-16, 10.00000000000000000, -7.250000000000000000 ) ) ;
#3311 = CARTESIAN_POINT ( 'NONE',  ( 1.553300858899105963, 14.56250000000000000, -7.250000000000000000 ) ) ;
#3312 = CARTESIAN_POINT ( 'NONE',  ( 6.770579566034212071, 2.743867526398027223, -34.56909192082981974 ) ) ;
#3313 = CARTESIAN_POINT ( 'NONE',  ( -4.238957102262124188, -1.739993903204167602E-15, -137.2930163777632799 ) ) ;
#3314 = CARTESIAN_POINT ( 'NONE',  ( 1.553300858899109516, 12.43750000000000000, 0.2499999999999993616 ) ) ;
#3315 = VECTOR ( 'NONE', #9535, 1000.000000000000000 ) ;
#3316 = CARTESIAN_POINT ( 'NONE',  ( -2.613481103162547114, 4.336808689942018722E-16, -113.0003292951173535 ) ) ;
#3317 = DIRECTION ( 'NONE',  ( 0.9984089457869175233, 7.979727989493312634E-17, -0.05638773778629511957 ) ) ;
#3318 = DIRECTION ( 'NONE',  ( -0.06144244613645849507, 0.7154473348115049092, -0.6959597236362767836 ) ) ;
#3319 = ORIENTED_EDGE ( 'NONE', *, *, #3760, .F. ) ;
#3320 = CARTESIAN_POINT ( 'NONE',  ( 8.875022474551933271, 4.581109498455814055, 5.628716231298513506 ) ) ;
#3321 = CARTESIAN_POINT ( 'NONE',  ( -3.249999999999999556, 0.2500000000000000000, -3.499999999999999556 ) ) ;
#3322 = CARTESIAN_POINT ( 'NONE',  ( -57.59976990480181058, 15.00000000000000000, -167.2044102620146759 ) ) ;
#3323 = CARTESIAN_POINT ( 'NONE',  ( -1.346194077712558945, 3.562500000000000888, -0.2500000000000002220 ) ) ;
#3324 = EDGE_LOOP ( 'NONE', ( #11552, #2018, #14248, #8449 ) ) ;
#3325 = DIRECTION ( 'NONE',  ( 0.000000000000000000, 0.000000000000000000, 1.000000000000000000 ) ) ;
#3326 = VECTOR ( 'NONE', #9516, 1000.000000000000000 ) ;
#3327 = CARTESIAN_POINT ( 'NONE',  ( -25.63598692233250986, 1.717341244404099410, -207.0184607745250105 ) ) ;
#3328 = DIRECTION ( 'NONE',  ( 0.000000000000000000, 0.000000000000000000, 1.000000000000000000 ) ) ;
#3329 = CARTESIAN_POINT ( 'NONE',  ( -4.781971238369687960, 5.000000000000000888, -110.8602639898370654 ) ) ;
#3330 = CARTESIAN_POINT ( 'NONE',  ( 3.249999999999998224, 11.18750000000000178, -4.846194077712561388 ) ) ;
#3331 = CARTESIAN_POINT ( 'NONE',  ( 4.413686865555820127, 8.673617379884035472E-16, -104.6754972201258624 ) ) ;
#3332 = CARTESIAN_POINT ( 'NONE',  ( -3.750000000000000000, 2.812500000000000444, -5.053300858899105741 ) ) ;
#3333 = CIRCLE ( 'NONE', #125, 5.000000000000001776 ) ;
#3334 = CARTESIAN_POINT ( 'NONE',  ( 6.122889832264990062, 15.00000000000000000, 5.281130614573720905 ) ) ;
#3335 = CARTESIAN_POINT ( 'NONE',  ( 5.000000000000000888, 15.00000000000000000, -100.6237003951525679 ) ) ;
#3336 = CARTESIAN_POINT ( 'NONE',  ( -6.351131181362492661, 10.00000000000000533, -118.7647174387982290 ) ) ;
#3337 = CARTESIAN_POINT ( 'NONE',  ( 10.87549112447535293, 2.099999999999148770, 58.60001680419858161 ) ) ;
#3338 = CARTESIAN_POINT ( 'NONE',  ( 2.298097038856278473, 9.625000000000000000, -5.798097038856279362 ) ) ;
#3339 = DIRECTION ( 'NONE',  ( 0.000000000000000000, 0.000000000000000000, -1.000000000000000000 ) ) ;
#3340 = DIRECTION ( 'NONE',  ( 0.000000000000000000, 1.000000000000000000, 0.000000000000000000 ) ) ;
#3341 = ORIENTED_EDGE ( 'NONE', *, *, #13116, .T. ) ;
#3342 = ORIENTED_EDGE ( 'NONE', *, *, #7997, .F. ) ;
#3343 = CARTESIAN_POINT ( 'NONE',  ( 3.254529015745487808, 4.000000000000000000, -173.6235312550020353 ) ) ;
#3344 = CARTESIAN_POINT ( 'NONE',  ( -2.651650429449553314, 6.375000000000000888, -6.151650429449552426 ) ) ;
#3345 = CARTESIAN_POINT ( 'NONE',  ( 0.000000000000000000, 1.500000000000000222, 0.2499999999999998057 ) ) ;
#3346 = CARTESIAN_POINT ( 'NONE',  ( 9.939878312292623974, 9.999999999999998224, -115.2320631035898373 ) ) ;
#3347 = EDGE_LOOP ( 'NONE', ( #10939, #15172, #426 ) ) ;
#3348 = CARTESIAN_POINT ( 'NONE',  ( 3.249999999999998224, 2.187500000000000000, -4.846194077712561388 ) ) ;
#3349 = EDGE_CURVE ( 'NONE', #4658, #10866, #4523, .T. ) ;
#3350 = CARTESIAN_POINT ( 'NONE',  ( -57.71664061942946233, 15.00000000000000000, -153.6990377947844593 ) ) ;
#3351 = CARTESIAN_POINT ( 'NONE',  ( -14.50484797826036321, 7.499999999999991118, -90.38469341974051474 ) ) ;
#3352 = ADVANCED_FACE ( 'NONE', ( #5450 ), #822, .F. ) ;
#3353 = CARTESIAN_POINT ( 'NONE',  ( 2.298097038856279362, 3.875000000000000000, -1.201902961143720860 ) ) ;
#3354 = APPROVAL_ROLE ( '' ) ;
#3355 = FACE_OUTER_BOUND ( 'NONE', #14290, .T. ) ;
#3356 = PLANE ( 'NONE',  #2726 ) ;
#3357 = ORIENTED_EDGE ( 'NONE', *, *, #7611, .T. ) ;
#3358 = CARTESIAN_POINT ( 'NONE',  ( 25.59005225942203055, 2.055286875414667591, -137.2931158548774988 ) ) ;
#3359 = CARTESIAN_POINT ( 'NONE',  ( 3.249999999999999556, 12.75000000000000178, -3.500000000000000000 ) ) ;
#3360 = ORIENTED_EDGE ( 'NONE', *, *, #12050, .T. ) ;
#3361 = ORIENTED_EDGE ( 'NONE', *, *, #11584, .F. ) ;
#3362 = CARTESIAN_POINT ( 'NONE',  ( -1.553300858899107073, 8.937500000000000000, -7.249999999999999112 ) ) ;
#3363 = CARTESIAN_POINT ( 'NONE',  ( -0.3675725891509493137, 0.000000000000000000, -0.3389548520155291622 ) ) ;
#3364 = CARTESIAN_POINT ( 'NONE',  ( 2.651650429449552870, 1.124999999999999778, -6.151650429449555091 ) ) ;
#3365 = CARTESIAN_POINT ( 'NONE',  ( -3.249999999999999556, 7.750000000000000888, -3.500000000000000000 ) ) ;
#3366 = ORIENTED_EDGE ( 'NONE', *, *, #4696, .F. ) ;
#3367 = FACE_OUTER_BOUND ( 'NONE', #10909, .T. ) ;
#3368 = CARTESIAN_POINT ( 'NONE',  ( 1.346194077712558057, 1.562500000000000000, -6.750000000000000000 ) ) ;
#3369 = CARTESIAN_POINT ( 'NONE',  ( 1.553300858899108849, 6.937500000000000000, 0.2499999999999993616 ) ) ;
#3370 = CARTESIAN_POINT ( 'NONE',  ( -25.22011045336418533, 0.8049789667763997958, -204.9699801733243874 ) ) ;
#3371 = EDGE_CURVE ( 'NONE', #1192, #5516, #8622, .T. ) ;
#3372 = EDGE_CURVE ( 'NONE', #6985, #13571, #4844, .T. ) ;
#3373 = PERSON_AND_ORGANIZATION ( #3176, #3020 ) ;
#3374 = EDGE_CURVE ( 'NONE', #15130, #10045, #8634, .T. ) ;
#3375 = CARTESIAN_POINT ( 'NONE',  ( -44.21823081166466096, 15.00000000000000000, -145.3603131190973272 ) ) ;
#3376 = CIRCLE ( 'NONE', #9101, 16.00000000006737721 ) ;
#3377 = ORIENTED_EDGE ( 'NONE', *, *, #7503, .T. ) ;
#3378 = CARTESIAN_POINT ( 'NONE',  ( -3.249999999999999556, 6.750000000000000888, -3.500000000000000000 ) ) ;
#3379 = CARTESIAN_POINT ( 'NONE',  ( 20.87131526946579285, 0.000000000000000000, -138.9752963459259547 ) ) ;
#3380 = CARTESIAN_POINT ( 'NONE',  ( 1.553300858899109071, 9.437500000000003553, 0.2499999999999989175 ) ) ;
#3381 = CIRCLE ( 'NONE', #12020, 6.000000000000002665 ) ;
#3382 = CARTESIAN_POINT ( 'NONE',  ( -29.69515346086422980, 5.000000000000000000, -156.7390981038715836 ) ) ;
#3383 = CARTESIAN_POINT ( 'NONE',  ( -65.55349497823009131, 14.94604455468336468, -187.0977264243838647 ) ) ;
#3384 = CARTESIAN_POINT ( 'NONE',  ( -0.3766621274091715987, -0.1687972351630583345, 0.1491815183709511161 ) ) ;
#3385 = CARTESIAN_POINT ( 'NONE',  ( 2.298097038856278029, 0.1250000000000001110, -5.798097038856279362 ) ) ;
#3386 = CARTESIAN_POINT ( 'NONE',  ( -4.090890948359609425, 15.00000000000000000, -103.1929727064838289 ) ) ;
#3387 = EDGE_CURVE ( 'NONE', #3600, #882, #2597, .T. ) ;
#3388 = DATE_AND_TIME ( #12977, #7460 ) ;
#3389 = CC_DESIGN_PERSON_AND_ORGANIZATION_ASSIGNMENT ( #9327, #2298, ( #11824 ) ) ;
#3390 = LINE ( 'NONE', #8100, #15195 ) ;
#3391 = VERTEX_POINT ( 'NONE', #3131 ) ;
#3392 = CARTESIAN_POINT ( 'NONE',  ( -29.21839114985998975, -1.098965884223355800E-12, -199.4123269880084024 ) ) ;
#3393 = CARTESIAN_POINT ( 'NONE',  ( -1.346194077712559167, 4.437500000000001776, -6.749999999999999112 ) ) ;
#3394 =( BOUNDED_SURFACE ( )  B_SPLINE_SURFACE ( 3, 1, ( 
 ( #13482, #6655 ),
 ( #2882, #1712 ),
 ( #11366, #10063 ),
 ( #12376, #5345 ) ),
 .UNSPECIFIED., .F., .F., .T. ) 
 B_SPLINE_SURFACE_WITH_KNOTS ( ( 4, 4 ),
 ( 2, 2 ),
 ( 0.000000000000000000, 1.000000000000000000 ),
 ( 0.000000000000000000, 1.000000000000000000 ),
 .UNSPECIFIED. ) 
 GEOMETRIC_REPRESENTATION_ITEM ( )  RATIONAL_B_SPLINE_SURFACE ( (
 ( 1.000000000000000000, 1.000000000000000000),
 ( 0.9999959457513183381, 0.9999959457513183381),
 ( 0.9999959457513183381, 0.9999959457513183381),
 ( 1.000000000000000000, 1.000000000000000000) ) ) 
 REPRESENTATION_ITEM ( '' )  SURFACE ( )  );
#3395 = CARTESIAN_POINT ( 'NONE',  ( -66.60702730184040377, 15.00000000000000000, -191.5456185926130956 ) ) ;
#3396 = CARTESIAN_POINT ( 'NONE',  ( -3.249999999999999112, 0.8125000000000001110, -4.846194077712558723 ) ) ;
#3397 = ORIENTED_EDGE ( 'NONE', *, *, #12408, .T. ) ;
#3398 = CARTESIAN_POINT ( 'NONE',  ( 4.011956498685772310, 5.000000000000001776, -134.9775950754472831 ) ) ;
#3399 = CARTESIAN_POINT ( 'NONE',  ( 2.850044070969222521, 5.000000000000000888, -103.0233998225063345 ) ) ;
#3400 = CARTESIAN_POINT ( 'NONE',  ( 8.875781042498779527, 10.69239977982764778, 5.593959306807169796 ) ) ;
#3401 = CARTESIAN_POINT ( 'NONE',  ( -3.886960648222041021E-10, 8.673617379884035472E-16, -101.1952717268999891 ) ) ;
#3402 = CARTESIAN_POINT ( 'NONE',  ( 2.298097038856279362, 11.37500000000000178, -1.201902961143720860 ) ) ;
#3403 = DIRECTION ( 'NONE',  ( 1.000000000000000000, 0.000000000000000000, 0.000000000000000000 ) ) ;
#3404 = CARTESIAN_POINT ( 'NONE',  ( -3.749999999999999556, 1.750000000000000222, -3.499999999999999112 ) ) ;
#3405 = FACE_OUTER_BOUND ( 'NONE', #10616, .T. ) ;
#3406 = CARTESIAN_POINT ( 'NONE',  ( -8.853589897535512065, 10.68297945906494029, -105.4984887282087982 ) ) ;
#3407 = DIRECTION ( 'NONE',  ( 0.000000000000000000, 0.000000000000000000, -1.000000000000000000 ) ) ;
#3408 = CARTESIAN_POINT ( 'NONE',  ( -2.238468823239509131, 7.379999999999995453, -42.41179034119947744 ) ) ;
#3409 = CARTESIAN_POINT ( 'NONE',  ( -3.249999999999999556, 12.31250000000000000, -4.846194077712557835 ) ) ;
#3410 = CARTESIAN_POINT ( 'NONE',  ( -6.619426566176021431, 14.36547257068670724, -103.8764596943030654 ) ) ;
#3411 = DIRECTION ( 'NONE',  ( 0.000000000000000000, 0.000000000000000000, -1.000000000000000000 ) ) ;
#3412 = ORIENTED_EDGE ( 'NONE', *, *, #10907, .F. ) ;
#3413 = EDGE_LOOP ( 'NONE', ( #7446, #2542, #7270 ) ) ;
#3414 = CARTESIAN_POINT ( 'NONE',  ( 9.032650406499481477, 4.000000000000000000, -169.1646757747120375 ) ) ;
#3415 = CARTESIAN_POINT ( 'NONE',  ( -1.553300858899107295, 6.437500000000000888, -7.250000000000000000 ) ) ;
#3416 = CARTESIAN_POINT ( 'NONE',  ( 2.651650429449553314, 3.375000000000000444, -0.8483495705504476847 ) ) ;
#3417 = CARTESIAN_POINT ( 'NONE',  ( 4.586790536108142469, 15.00000000000000000, -116.5616331786029036 ) ) ;
#3418 = ORIENTED_EDGE ( 'NONE', *, *, #10609, .F. ) ;
#3419 = CARTESIAN_POINT ( 'NONE',  ( -1.346194077712559389, 14.06249999999999822, -0.2500000000000002220 ) ) ;
#3420 = CARTESIAN_POINT ( 'NONE',  ( -52.65879960150161310, 15.00000000000000000, -146.8206079635090191 ) ) ;
#3421 = CARTESIAN_POINT ( 'NONE',  ( 47.94704514886957014, 2.100000000000000089, 60.33052086138381043 ) ) ;
#3422 = SHAPE_REPRESENTATION_RELATIONSHIP ( 'NONE' , 'NONE' ,  #7636, #9451 ) ;
#3423 = CARTESIAN_POINT ( 'NONE',  ( 2.298097038856278473, 4.625000000000000000, -5.798097038856279362 ) ) ;
#3424 = ITEM_DEFINED_TRANSFORMATION ( 'NONE', 'NONE', #14132,  #9419 ) ;
#3425 = DIRECTION ( 'NONE',  ( 0.000000000000000000, 0.000000000000000000, -1.000000000000000000 ) ) ;
#3426 = DIRECTION ( 'NONE',  ( 0.000000000000000000, 0.000000000000000000, -1.000000000000000000 ) ) ;
#3427 = ORIENTED_EDGE ( 'NONE', *, *, #3454, .F. ) ;
#3428 = CARTESIAN_POINT ( 'NONE',  ( -4.567589802617025185, 14.99999999999999822, -125.7656343796584082 ) ) ;
#3429 = CARTESIAN_POINT ( 'NONE',  ( 1.346194077712558279, 11.56250000000000000, -6.750000000000000000 ) ) ;
#3430 = EDGE_LOOP ( 'NONE', ( #13565, #9466, #1939 ) ) ;
#3431 = ADVANCED_FACE ( 'NONE', ( #5596 ), #3356, .T. ) ;
#3432 = EDGE_LOOP ( 'NONE', ( #10407, #1351, #13765, #12891 ) ) ;
#3433 = CARTESIAN_POINT ( 'NONE',  ( 0.000000000000000000, 8.500000000000000000, 0.2500000000000002220 ) ) ;
#3434 = CARTESIAN_POINT ( 'NONE',  ( -5.011228476432583179, 2.331468351712828833E-16, 8.417957015065626436 ) ) ;
#3435 = CARTESIAN_POINT ( 'NONE',  ( -3.750000000000000000, 7.687500000000000888, -1.946699141100893149 ) ) ;
#3436 = CARTESIAN_POINT ( 'NONE',  ( 2.298097038856278029, 5.125000000000000888, -5.798097038856279362 ) ) ;
#3437 = ORIENTED_EDGE ( 'NONE', *, *, #1294, .F. ) ;
#3438 = ADVANCED_FACE ( 'NONE', ( #743 ), #6904, .F. ) ;
#3439 = CARTESIAN_POINT ( 'NONE',  ( -1.499260709886190313, 15.00000000000162537, -106.0110764664949556 ) ) ;
#3440 = CARTESIAN_POINT ( 'NONE',  ( 3.249999999999999556, 3.750000000000000000, -3.500000000000000000 ) ) ;
#3441 = CARTESIAN_POINT ( 'NONE',  ( -2.651650429449552870, 5.125000000000000000, -0.8483495705504462414 ) ) ;
#3442 = FACE_OUTER_BOUND ( 'NONE', #2132, .T. ) ;
#3443 = CARTESIAN_POINT ( 'NONE',  ( -17.32624372123753886, 15.00000000000000000, -122.3796757791585321 ) ) ;
#3444 = CARTESIAN_POINT ( 'NONE',  ( 4.716951098700676859, -2.490287375297125294, -44.10818225254241298 ) ) ;
#3445 = DATE_AND_TIME ( #2213, #15069 ) ;
#3446 = CARTESIAN_POINT ( 'NONE',  ( 2.036468110357356309, 2.352429041693352207, -1.000000000000007772 ) ) ;
#3447 = CARTESIAN_POINT ( 'NONE',  ( 30.93967778936172053, 8.773889247172311556, -42.92540924734178986 ) ) ;
#3448 = LOCAL_TIME ( 12, 28, 20.00000000000000000, #4462 ) ;
#3449 = ORIENTED_EDGE ( 'NONE', *, *, #6759, .T. ) ;
#3450 = VECTOR ( 'NONE', #10927, 1000.000000000000000 ) ;
#3451 = CARTESIAN_POINT ( 'NONE',  ( -1.346194077712559167, 8.937500000000000000, -6.749999999999999112 ) ) ;
#3452 = EDGE_CURVE ( 'NONE', #14745, #5270, #12839, .T. ) ;
#3453 = DIRECTION ( 'NONE',  ( 0.08794243244723005948, 0.000000000000000000, 0.9961255586397049777 ) ) ;
#3454 = EDGE_CURVE ( 'NONE', #505, #1748, #6689, .T. ) ;
#3455 = CARTESIAN_POINT ( 'NONE',  ( -3.749999999999999556, 8.750000000000001776, -3.499999999999999112 ) ) ;
#3456 = CARTESIAN_POINT ( 'NONE',  ( 3.749999999999999556, 12.81250000000000178, -1.946699141100892261 ) ) ;
#3457 = CC_DESIGN_APPROVAL ( #6490, ( #10865 ) ) ;
#3458 = CARTESIAN_POINT ( 'NONE',  ( -65.84020878422680312, 15.11604966749248646, -201.7286952349428475 ) ) ;
#3459 = CARTESIAN_POINT ( 'NONE',  ( 0.000000000000000000, 4.000000000000000000, -2.000000000000000000 ) ) ;
#3460 = CARTESIAN_POINT ( 'NONE',  ( 1.553300858899105963, 13.06249999999999822, -7.250000000000000888 ) ) ;
#3461 = CIRCLE ( 'NONE', #14854, 3.500000000000013323 ) ;
#3462 = PLANE ( 'NONE',  #10696 ) ;
#3463 = AXIS2_PLACEMENT_3D ( 'NONE', #15028, #15182, #6662 ) ;
#3464 = APPROVAL_STATUS ( 'not_yet_approved' ) ;
#3465 = AXIS2_PLACEMENT_3D ( 'NONE', #687, #14769, #5392 ) ;
#3466 = DIRECTION ( 'NONE',  ( -0.000000000000000000, 1.000000000000000000, -0.000000000000000000 ) ) ;
#3467 = ORIENTED_EDGE ( 'NONE', *, *, #10014, .T. ) ;
#3468 = CARTESIAN_POINT ( 'NONE',  ( 8.935548306746156300, 5.000000000000000888, 2.855381328098106408 ) ) ;
#3469 = CARTESIAN_POINT ( 'NONE',  ( 2.298097038856278473, 2.625000000000000000, -5.798097038856279362 ) ) ;
#3470 = CARTESIAN_POINT ( 'NONE',  ( -53.33476332437127354, 15.00000000000000000, -169.8150382216088587 ) ) ;
#3471 = CIRCLE ( 'NONE', #2481, 3.000000000000010214 ) ;
#3472 = CARTESIAN_POINT ( 'NONE',  ( 3.249999999999998224, 8.312500000000003553, -2.153805922287439945 ) ) ;
#3473 = ORIENTED_EDGE ( 'NONE', *, *, #3761, .F. ) ;
#3474 = CARTESIAN_POINT ( 'NONE',  ( -5.808150136414201192, 9.999999999999998224, -117.3161822536842607 ) ) ;
#3475 = AXIS2_PLACEMENT_3D ( 'NONE', #4863, #2629, #7331 ) ;
#3476 = AXIS2_PLACEMENT_3D ( 'NONE', #12364, #12136, #10049 ) ;
#3477 = ADVANCED_FACE ( 'NONE', ( #6765 ), #7995, .T. ) ;
#3478 = CARTESIAN_POINT ( 'NONE',  ( -25.70034284263700286, 0.9795334954347006962, -205.5107766831865774 ) ) ;
#3479 = CARTESIAN_POINT ( 'NONE',  ( -5.445322652854981627, 5.900679960901947346E-16, -1.000000000000000000 ) ) ;
#3480 = CARTESIAN_POINT ( 'NONE',  ( -3.249999999999999112, 10.68750000000000178, -2.153805922287440833 ) ) ;
#3481 = DIRECTION ( 'NONE',  ( -0.02181900108494707127, 0.000000000000000000, 0.9997619372588931741 ) ) ;
#3482 = CARTESIAN_POINT ( 'NONE',  ( 3.749999999999999556, 1.250000000000000222, -3.500000000000000444 ) ) ;
#3483 = CARTESIAN_POINT ( 'NONE',  ( -0.3766621274091715987, -0.2374287473167014662, 0.07324965529007555765 ) ) ;
#3484 = AXIS2_PLACEMENT_3D ( 'NONE', #14211, #12898, #4699 ) ;
#3485 = FACE_BOUND ( 'NONE', #8055, .T. ) ;
#3486 =( BOUNDED_CURVE ( )  B_SPLINE_CURVE ( 3, ( #141, #2383, #10571, #7080 ),
 .UNSPECIFIED., .F., .T. ) 
 B_SPLINE_CURVE_WITH_KNOTS ( ( 4, 4 ),
 ( 4.712388980384687898, 4.907255421178649435 ),
 .UNSPECIFIED. ) 
 CURVE ( )  GEOMETRIC_REPRESENTATION_ITEM ( )  RATIONAL_B_SPLINE_CURVE ( ( 1.000000000000000000, 0.9968380917696022525, 0.9968380917696022525, 1.000000000000000000 ) ) 
 REPRESENTATION_ITEM ( '' )  );
#3487 = DIRECTION ( 'NONE',  ( 0.000000000000000000, -1.000000000000000000, 0.000000000000000000 ) ) ;
#3488 = CARTESIAN_POINT ( 'NONE',  ( 4.010609318860100636, 13.34515119446107612, 3.652314080085856229 ) ) ;
#3489 = CARTESIAN_POINT ( 'NONE',  ( 1.346194077712558057, 11.56249999999999822, -6.750000000000000000 ) ) ;
#3490 = VECTOR ( 'NONE', #8042, 1000.000000000000000 ) ;
#3491 = CARTESIAN_POINT ( 'NONE',  ( -9.203293576667494591, 10.68436263327555835, -104.6513152614200237 ) ) ;
#3492 = FACE_OUTER_BOUND ( 'NONE', #2184, .T. ) ;
#3493 = VERTEX_POINT ( 'NONE', #2424 ) ;
#3494 =( BOUNDED_CURVE ( )  B_SPLINE_CURVE ( 3, ( #11308, #13719, #8915, #13566 ),
 .UNSPECIFIED., .F., .F. ) 
 B_SPLINE_CURVE_WITH_KNOTS ( ( 4, 4 ),
 ( 5.855884514716120925, 5.964107263055466568 ),
 .UNSPECIFIED. ) 
 CURVE ( )  GEOMETRIC_REPRESENTATION_ITEM ( )  RATIONAL_B_SPLINE_CURVE ( ( 1.000000000000000000, 0.9990242245225531281, 0.9990242245225531281, 1.000000000000000000 ) ) 
 REPRESENTATION_ITEM ( '' )  );
#3495 = VERTEX_POINT ( 'NONE', #1266 ) ;
#3496 = DIRECTION ( 'NONE',  ( -0.000000000000000000, 1.000000000000000000, -0.000000000000000000 ) ) ;
#3497 = CARTESIAN_POINT ( 'NONE',  ( -3.749999999999999556, 5.187500000000001776, -1.946699141100892927 ) ) ;
#3498 = CARTESIAN_POINT ( 'NONE',  ( -1.553300858899106629, 3.562500000000000888, 0.2499999999999998335 ) ) ;
#3499 = CARTESIAN_POINT ( 'NONE',  ( 0.3766621274091715987, -0.2500000000000000000, 0.1491815183709511716 ) ) ;
#3500 = ORIENTED_EDGE ( 'NONE', *, *, #9690, .F. ) ;
#3501 = TOROIDAL_SURFACE ( 'NONE', #9172, 1.250000000000002220, 1.750000000000000000 ) ;
#3502 = CARTESIAN_POINT ( 'NONE',  ( -3.249999999999999556, 14.25000000000000000, -3.499999999999999556 ) ) ;
#3503 = CARTESIAN_POINT ( 'NONE',  ( -56.93825309396395085, 15.00000000000456346, -152.5131710536675200 ) ) ;
#3504 = CARTESIAN_POINT ( 'NONE',  ( 4.505624869885556549, 8.673617379884035472E-16, -107.9937432812489675 ) ) ;
#3505 = CARTESIAN_POINT ( 'NONE',  ( 3.249999999999999112, 3.812500000000000000, -2.153805922287439945 ) ) ;
#3506 = PERSON_AND_ORGANIZATION_ROLE ( 'classification_officer' ) ;
#3507 = B_SPLINE_CURVE_WITH_KNOTS ( 'NONE', 3,
 ( #12625, #12472, #5511, #1958, #8916, #11463, #3267, #810, #13645, #730, #3188, #11309, #3046, #6444, #6673, #8992 ),
 .UNSPECIFIED., .F., .F.,
 ( 4, 2, 2, 2, 2, 2, 2, 4 ),
 ( 0.0004752521799440825390, 0.007644733457695613091, 0.01122947409657133917, 0.01481421473544706699, 0.02198369601319844976, 0.02915317729094983254, 0.04349213984645259462, 0.05783110240195536711 ),
 .UNSPECIFIED. ) ;
#3508 = LOCAL_TIME ( 12, 28, 20.00000000000000000, #9840 ) ;
#3509 = PLANE ( 'NONE',  #6775 ) ;
#3510 = CARTESIAN_POINT ( 'NONE',  ( 9.410602039242014882, 1.734723475976807094E-15, -119.1126025278262972 ) ) ;
#3511 = VERTEX_POINT ( 'NONE', #7052 ) ;
#3512 = DIRECTION ( 'NONE',  ( 0.1564344650402314796, 0.000000000000000000, 0.9876883405951375483 ) ) ;
#3513 = CARTESIAN_POINT ( 'NONE',  ( -2.298097038856278473, 14.12500000000000000, -1.201902961143720416 ) ) ;
#3514 = ORIENTED_EDGE ( 'NONE', *, *, #5177, .F. ) ;
#3515 = EDGE_LOOP ( 'NONE', ( #11061, #5637, #13314, #3210, #2265 ) ) ;
#3516 = CARTESIAN_POINT ( 'NONE',  ( -8.060080686208022982, 9.999999999999998224, -91.29668298688132211 ) ) ;
#3517 = CARTESIAN_POINT ( 'NONE',  ( 2.651650429449552870, 6.125000000000000000, -6.151650429449555091 ) ) ;
#3518 = CARTESIAN_POINT ( 'NONE',  ( 3.249999999999998224, 8.312500000000003553, -2.153805922287439945 ) ) ;
#3519 = ORIENTED_EDGE ( 'NONE', *, *, #14418, .F. ) ;
#3520 = CARTESIAN_POINT ( 'NONE',  ( 5.000000000000000000, 14.99999999999999822, -100.6237003951525537 ) ) ;
#3521 = CARTESIAN_POINT ( 'NONE',  ( -3.249999999999999556, 2.187500000000000444, -2.153805922287440833 ) ) ;
#3522 = CARTESIAN_POINT ( 'NONE',  ( 0.000000000000000000, 9.000000000000001776, 0.2500000000000002220 ) ) ;
#3523 = CARTESIAN_POINT ( 'NONE',  ( -1.500000000000000000, 4.500000000000000888, -0.2499999999999997780 ) ) ;
#3524 = CIRCLE ( 'NONE', #4033, 3.000000000000002665 ) ;
#3525 = CARTESIAN_POINT ( 'NONE',  ( 0.000000000000000000, 15.00000000000000000, 0.2500000000000002220 ) ) ;
#3526 = DATE_AND_TIME ( #8236, #5182 ) ;
#3527 = ADVANCED_FACE ( 'NONE', ( #2584 ), #10985, .T. ) ;
#3528 = DIRECTION ( 'NONE',  ( 0.5205261093005589812, 0.000000000000000000, -0.8538457527776445177 ) ) ;
#3529 = ORIENTED_EDGE ( 'NONE', *, *, #6781, .T. ) ;
#3530 = CARTESIAN_POINT ( 'NONE',  ( -2.298097038856279362, 8.875000000000000000, -5.798097038856278473 ) ) ;
#3531 = CARTESIAN_POINT ( 'NONE',  ( -9.030574454602202650, 2.490287375297125294, -34.97919997656153157 ) ) ;
#3532 = ADVANCED_BREP_SHAPE_REPRESENTATION ( '', ( #7543, #9419 ), #2511 ) ;
#3533 = TOROIDAL_SURFACE ( 'NONE', #11192, 9.800000000000245848, 5.000000000000000000 ) ;
#3534 = CARTESIAN_POINT ( 'NONE',  ( 1.553300858899109071, 12.43750000000000000, 0.2499999999999989175 ) ) ;
#3535 = CARTESIAN_POINT ( 'NONE',  ( -6.288157641191917335, 6.000000000000000000, -124.9981450708252595 ) ) ;
#3536 = CARTESIAN_POINT ( 'NONE',  ( -64.63541926112564795, 14.99927084828137858, -184.1902271030175484 ) ) ;
#3537 = CARTESIAN_POINT ( 'NONE',  ( -2.580341218501653433, 0.4558749503568839123, -137.7136442480489222 ) ) ;
#3538 = CARTESIAN_POINT ( 'NONE',  ( 2.651650429449554203, 14.37500000000000000, -0.8483495705504471296 ) ) ;
#3539 = CARTESIAN_POINT ( 'NONE',  ( -2.986019729822490643, 4.336808689942016750E-16, -116.5136792814622879 ) ) ;
#3540 = CALENDAR_DATE ( 2026, 8, 10 ) ;
#3541 = EDGE_CURVE ( 'NONE', #7777, #114, #1501, .T. ) ;
#3542 = CARTESIAN_POINT ( 'NONE',  ( 3.235167919141236137, 15.00000000000000000, -114.6791120453068373 ) ) ;
#3543 = AXIS2_PLACEMENT_3D ( 'NONE', #8260, #2702, #7401 ) ;
#3544 = CARTESIAN_POINT ( 'NONE',  ( -3.520407287333057855, 7.379999999999995453, -45.56125597433126018 ) ) ;
#3545 = CIRCLE ( 'NONE', #13445, 3.500000000000000000 ) ;
#3546 = ORIENTED_EDGE ( 'NONE', *, *, #6856, .F. ) ;
#3547 = CARTESIAN_POINT ( 'NONE',  ( 6.122889832264990062, 5.000000000000000888, 5.281130614573720017 ) ) ;
#3548 = CARTESIAN_POINT ( 'NONE',  ( 3.249999999999998668, 1.687500000000000000, -4.846194077712560500 ) ) ;
#3549 = CARTESIAN_POINT ( 'NONE',  ( -7.316781067255146098, 0.05734158317339200367, -104.2569854988662570 ) ) ;
#3550 = CARTESIAN_POINT ( 'NONE',  ( -3.249999999999999556, 8.750000000000000000, -3.500000000000000000 ) ) ;
#3551 = ORIENTED_EDGE ( 'NONE', *, *, #6202, .T. ) ;
#3552 = CARTESIAN_POINT ( 'NONE',  ( -1.457387361610950727, 15.00000000000000000, -106.9488561393970940 ) ) ;
#3553 = DIRECTION ( 'NONE',  ( -0.9961255586397056438, 0.000000000000000000, 0.08794243244722428632 ) ) ;
#3554 = CARTESIAN_POINT ( 'NONE',  ( 6.491365067585770809, 15.00000000000000000, 0.2705411889128687131 ) ) ;
#3555 = LINE ( 'NONE', #1089, #3715 ) ;
#3556 = AXIS2_PLACEMENT_3D ( 'NONE', #4001, #598, #2910 ) ;
#3557 = CARTESIAN_POINT ( 'NONE',  ( 1.346194077712561166, 11.43750000000000178, -0.2500000000000011102 ) ) ;
#3558 = APPROVAL ( #10610, 'UNKNOWN' ) ;
#3559 = CARTESIAN_POINT ( 'NONE',  ( 1.553300858899108849, 6.937500000000000000, 0.2499999999999993616 ) ) ;
#3560 = DIRECTION ( 'NONE',  ( -0.02181900108494707127, 8.601065436648711846E-18, 0.9997619372588932851 ) ) ;
#3561 = CARTESIAN_POINT ( 'NONE',  ( -3.749999999999999556, 0.7500000000000001110, -3.499999999999999112 ) ) ;
#3562 = DIRECTION ( 'NONE',  ( -0.9961255586397055328, 0.000000000000000000, 0.08794243244722428632 ) ) ;
#3563 = CARTESIAN_POINT ( 'NONE',  ( 0.01496453197139708223, 0.000000000000000000, 5.196130874293197088 ) ) ;
#3564 = EDGE_CURVE ( 'NONE', #2807, #14091, #6212, .T. ) ;
#3565 = EDGE_CURVE ( 'NONE', #14271, #8293, #9771, .T. ) ;
#3566 = CARTESIAN_POINT ( 'NONE',  ( 1.114947364559093712, 6.000000000000000000, -139.4079432275550232 ) ) ;
#3567 = ADVANCED_FACE ( 'NONE', ( #13334 ), #7910, .T. ) ;
#3568 = CARTESIAN_POINT ( 'NONE',  ( 14.67769753127737253, 0.000000000000000000, 60.42036742134819605 ) ) ;
#3569 = CARTESIAN_POINT ( 'NONE',  ( -2.298097038856278473, 11.12500000000000000, -1.201902961143720416 ) ) ;
#3570 = CIRCLE ( 'NONE', #13702, 3.500000000000000000 ) ;
#3571 = CARTESIAN_POINT ( 'NONE',  ( -4.421378549306751893, 14.99999999999999822, -103.2781497068736059 ) ) ;
#3572 = CARTESIAN_POINT ( 'NONE',  ( -65.02458175624013847, 14.37806382103629588, -196.6750733491710719 ) ) ;
#3573 = ORIENTED_EDGE ( 'NONE', *, *, #4309, .T. ) ;
#3574 = ORIENTED_EDGE ( 'NONE', *, *, #5829, .F. ) ;
#3575 = CARTESIAN_POINT ( 'NONE',  ( -5.763540231036513362, 2.500000000000000444, -109.7236846929843210 ) ) ;
#3576 = CARTESIAN_POINT ( 'NONE',  ( 4.641633639902737585, 8.673617379884035472E-16, -171.4570495182728394 ) ) ;
#3577 = CARTESIAN_POINT ( 'NONE',  ( 3.749999999999999112, 5.812500000000000000, -1.946699141100892039 ) ) ;
#3578 = CARTESIAN_POINT ( 'NONE',  ( -3.749999999999999556, 4.750000000000000000, -3.499999999999999112 ) ) ;
#3579 = CC_DESIGN_PERSON_AND_ORGANIZATION_ASSIGNMENT ( #9711, #10862, ( #12881 ) ) ;
#3580 = CARTESIAN_POINT ( 'NONE',  ( 0.000000000000000000, 4.000000000000000000, 0.000000000000000000 ) ) ;
#3581 = VERTEX_POINT ( 'NONE', #991 ) ;
#3582 = CARTESIAN_POINT ( 'NONE',  ( -8.207841483266339111, 1.782382842934248757, -115.8806436028926754 ) ) ;
#3583 = CARTESIAN_POINT ( 'NONE',  ( -3.249999999999999556, 13.18749999999999822, -2.153805922287440833 ) ) ;
#3584 =( BOUNDED_SURFACE ( )  B_SPLINE_SURFACE ( 3, 2, ( 
 ( #5884, #6896, #4817 ),
 ( #13015, #10386, #5816 ),
 ( #27, #2273, #7113 ),
 ( #1261, #10686, #15199 ),
 ( #11694, #3420, #4663 ),
 ( #9299, #8132, #104 ),
 ( #9530, #4517, #9369 ),
 ( #14101, #3503, #9224 ),
 ( #13953, #3350, #12786 ),
 ( #12234, #1340, #14328 ),
 ( #3894, #8593, #3732 ),
 ( #12154, #2500, #8355 ),
 ( #6044, #14570, #7436 ),
 ( #7515, #5204, #13328 ),
 ( #13083, #14496, #8438 ),
 ( #2731, #1490, #1571 ),
 ( #6205, #7195, #11915 ),
 ( #2657, #1417, #10762 ),
 ( #6122, #13252, #415 ),
 ( #10835, #3654, #6284 ),
 ( #12070, #9601, #2814 ),
 ( #9838, #11993, #10920 ),
 ( #11000, #13169, #1646 ),
 ( #489, #2579, #5123 ),
 ( #11072, #6360, #9918 ),
 ( #3970, #7279, #7357 ),
 ( #337, #8676, #5051 ),
 ( #9766, #13409, #179 ),
 ( #4889, #254, #4969 ),
 ( #9684, #14416, #3814 ),
 ( #8518, #7665, #3177 ),
 ( #11150, #4052, #10141 ),
 ( #13710, #3109, #12462 ),
 ( #12303, #12381, #13634 ),
 ( #7820, #8904, #1948 ),
 ( #6661, #14651, #1880 ),
 ( #11374, #12534, #799 ),
 ( #3036, #5501, #1802 ) ),
 .UNSPECIFIED., .F., .F., .F. ) 
 B_SPLINE_SURFACE_WITH_KNOTS ( ( 4, 2, 2, 2, 2, 2, 2, 2, 2, 2, 2, 2, 2, 2, 2, 2, 2, 2, 4 ),
 ( 3, 3 ),
 ( 0.08381559250741665856, 0.08776888376050354101, 0.09172217501359040959, 0.09567546626667727816, 0.09962875751976416061, 0.1075353400259379255, 0.1154419225321116765, 0.1233485050382854276, 0.1273017962913723100, 0.1312550875444591925, 0.1352083787975460749, 0.1371850244240895300, 0.1391616700506329574, 0.1411383156771763847, 0.1431149613037198121, 0.1441032841169915257, 0.1450916069302632394, 0.1460799297435349531, 0.1470682525568066945 ),
 ( 0.000000000000000000, 1.000000000000000000 ),
 .UNSPECIFIED. ) 
 GEOMETRIC_REPRESENTATION_ITEM ( )  RATIONAL_B_SPLINE_SURFACE ( (
 ( 1.000000000000000000, 0.7071067811865475727, 1.000000000000000000),
 ( 1.000000000000000000, 0.7071067811865475727, 1.000000000000000000),
 ( 1.000000000000000000, 0.7071067811865477948, 1.000000000000000000),
 ( 1.000000000000000000, 0.7071067811865477948, 1.000000000000000000),
 ( 1.000000000000000000, 0.7071067811865475727, 1.000000000000000000),
 ( 1.000000000000000000, 0.7071067811865475727, 1.000000000000000000),
 ( 1.000000000000000000, 0.7071067811865475727, 1.000000000000000000),
 ( 1.000000000000000000, 0.7071067811865475727, 1.000000000000000000),
 ( 1.000000000000000000, 0.7071067811865475727, 1.000000000000000000),
 ( 1.000000000000000000, 0.7071067811865475727, 1.000000000000000000),
 ( 1.000000000000000000, 0.7071067811865471286, 1.000000000000000000),
 ( 1.000000000000000000, 0.7071067811865471286, 1.000000000000000000),
 ( 1.000000000000000000, 0.7071067811865475727, 1.000000000000000000),
 ( 1.000000000000000000, 0.7071067811865475727, 1.000000000000000000),
 ( 1.000000000000000000, 0.7071067811865471286, 1.000000000000000000),
 ( 1.000000000000000000, 0.7071067811865471286, 1.000000000000000000),
 ( 1.000000000000000000, 0.7071067811865475727, 1.000000000000000000),
 ( 1.000000000000000000, 0.7071067811865475727, 1.000000000000000000),
 ( 1.000000000000000000, 0.7071067811865477948, 1.000000000000000000),
 ( 1.000000000000000000, 0.7071067811865477948, 1.000000000000000000),
 ( 1.000000000000000000, 0.7071067811865475727, 1.000000000000000000),
 ( 1.000000000000000000, 0.7071067811865475727, 1.000000000000000000),
 ( 1.000000000000000000, 0.7071067811865475727, 1.000000000000000000),
 ( 1.000000000000000000, 0.7071067811865475727, 1.000000000000000000),
 ( 1.000000000000000000, 0.7071067811865475727, 1.000000000000000000),
 ( 1.000000000000000000, 0.7071067811865475727, 1.000000000000000000),
 ( 1.000000000000000000, 0.7071067811865475727, 1.000000000000000000),
 ( 1.000000000000000000, 0.7071067811865475727, 1.000000000000000000),
 ( 1.000000000000000000, 0.7071067811865475727, 1.000000000000000000),
 ( 1.000000000000000000, 0.7071067811865475727, 1.000000000000000000),
 ( 1.000000000000000000, 0.7071067811865475727, 1.000000000000000000),
 ( 1.000000000000000000, 0.7071067811865475727, 1.000000000000000000),
 ( 1.000000000000000000, 0.7071067811865475727, 1.000000000000000000),
 ( 1.000000000000000000, 0.7071067811865475727, 1.000000000000000000),
 ( 1.000000000000000000, 0.7071067811865466846, 1.000000000000000000),
 ( 1.000000000000000000, 0.7071067811865466846, 1.000000000000000000),
 ( 1.000000000000000000, 0.7071067811865465735, 1.000000000000000000),
 ( 1.000000000000000000, 0.7071067811865465735, 1.000000000000000000) ) ) 
 REPRESENTATION_ITEM ( '' )  SURFACE ( )  );
#3585 = CARTESIAN_POINT ( 'NONE',  ( 1.727947212398772889E-15, 5.000000000000000888, -101.3854116612075558 ) ) ;
#3586 = CARTESIAN_POINT ( 'NONE',  ( 3.495361625530554406, 8.673617379884035472E-16, -116.4903051220812245 ) ) ;
#3587 = CARTESIAN_POINT ( 'NONE',  ( 3.249999999999998668, 5.687500000000000000, -4.846194077712560500 ) ) ;
#3588 = CALENDAR_DATE ( 2026, 8, 10 ) ;
#3589 =( BOUNDED_SURFACE ( )  B_SPLINE_SURFACE ( 3, 3, ( 
 ( #11075, #2890, #5426, #492, #14733, #12385, #1884 ),
 ( #722, #5286, #803, #9061, #10148, #6592, #6664 ),
 ( #14882, #8762, #3039, #12307, #4279, #6436, #651 ),
 ( #8984, #9998, #1806, #5504, #2959, #11380, #6363 ) ),
 .UNSPECIFIED., .F., .F., .F. ) 
 B_SPLINE_SURFACE_WITH_KNOTS ( ( 4, 4 ),
 ( 4, 3, 4 ),
 ( 0.000000000000000000, 1.000000000000000000 ),
 ( 0.000000000000000000, 0.5000000000000000000, 1.000000000000000000 ),
 .UNSPECIFIED. ) 
 GEOMETRIC_REPRESENTATION_ITEM ( )  RATIONAL_B_SPLINE_SURFACE ( (
 ( 1.000000000000000000, 0.7662986988867873661, 0.7662986988867873661, 1.000000000000000000, 0.7662986988867873661, 0.7662986988867873661, 1.000000000000000000),
 ( 0.6468719831415912225, 0.4956971590277172157, 0.4956971590277172157, 0.6468719831415912225, 0.4956971590277172157, 0.4956971590277172157, 0.6468719831415912225),
 ( 0.6468719831415912225, 0.4956971590277172157, 0.4956971590277172157, 0.6468719831415912225, 0.4956971590277172157, 0.4956971590277172157, 0.6468719831415912225),
 ( 1.000000000000000000, 0.7662986988867873661, 0.7662986988867873661, 1.000000000000000000, 0.7662986988867873661, 0.7662986988867873661, 1.000000000000000000) ) ) 
 REPRESENTATION_ITEM ( '' )  SURFACE ( )  );
#3590 = DIRECTION ( 'NONE',  ( 0.000000000000000000, -0.000000000000000000, -1.000000000000000000 ) ) ;
#3591 = CARTESIAN_POINT ( 'NONE',  ( 8.694046762359278091, 4.317799523304588693E-13, -116.9683691484218429 ) ) ;
#3592 = ORIENTED_EDGE ( 'NONE', *, *, #2913, .F. ) ;
#3593 = FACE_OUTER_BOUND ( 'NONE', #6576, .T. ) ;
#3594 = LINE ( 'NONE', #7122, #3228 ) ;
#3595 = ORIENTED_EDGE ( 'NONE', *, *, #3850, .F. ) ;
#3596 = ORIENTED_EDGE ( 'NONE', *, *, #162, .T. ) ;
#3597 = LINE ( 'NONE', #5896, #1320 ) ;
#3598 = CARTESIAN_POINT ( 'NONE',  ( 1.553300858899109516, 5.437500000000000888, 0.2499999999999993616 ) ) ;
#3599 = CARTESIAN_POINT ( 'NONE',  ( -3.249999999999999112, 4.687500000000000888, -2.153805922287440833 ) ) ;
#3600 = VERTEX_POINT ( 'NONE', #15000 ) ;
#3601 = CARTESIAN_POINT ( 'NONE',  ( 6.146364248477357961, 12.22024339317073505, 4.771788172891424651 ) ) ;
#3602 = CARTESIAN_POINT ( 'NONE',  ( 1.346194077712558057, 2.562500000000000444, -6.750000000000000000 ) ) ;
#3603 = CARTESIAN_POINT ( 'NONE',  ( -5.111334017457858536, 2.499999999999999556, -113.2220991196416549 ) ) ;
#3604 = CARTESIAN_POINT ( 'NONE',  ( -34.54324019596916173, 9.999999999999998224, -156.1716796081745429 ) ) ;
#3605 = CARTESIAN_POINT ( 'NONE',  ( 6.410190855677554644, 14.99999999999999645, -118.0482597935656059 ) ) ;
#3606 = DATE_AND_TIME ( #12888, #493 ) ;
#3607 = CARTESIAN_POINT ( 'NONE',  ( 2.691563203584910635, 1.625551886426497727, -1.000000000000001110 ) ) ;
#3608 = ORIENTED_EDGE ( 'NONE', *, *, #12050, .F. ) ;
#3609 = CARTESIAN_POINT ( 'NONE',  ( 5.137957026085652856, 1.921202954650395478, -45.03258396026100030 ) ) ;
#3610 = CARTESIAN_POINT ( 'NONE',  ( -2.651650429449552870, 13.62500000000000000, -0.8483495705504467965 ) ) ;
#3611 = DIRECTION ( 'NONE',  ( 1.000000000000000000, 0.000000000000000000, 0.000000000000000000 ) ) ;
#3612 = CARTESIAN_POINT ( 'NONE',  ( -63.28143670021790967, 10.89016550017335128, -203.4568824459457232 ) ) ;
#3613 = CARTESIAN_POINT ( 'NONE',  ( 0.07898452467418404233, 2.651103404268615460, -138.2779449578589208 ) ) ;
#3614 = CARTESIAN_POINT ( 'NONE',  ( 2.298097038856278029, 4.125000000000000000, -5.798097038856279362 ) ) ;
#3615 = CARTESIAN_POINT ( 'NONE',  ( 10.61533446930841329, 2.427390659569241826, -106.1975553300598847 ) ) ;
#3616 = MECHANICAL_CONTEXT ( 'NONE', #81, 'mechanical' ) ;
#3617 = PRODUCT ( 'BladeScrew_Predeterminado', 'BladeScrew_Predeterminado', '', ( #6000 ) ) ;
#3618 = CARTESIAN_POINT ( 'NONE',  ( -9.240119717576689595, 15.00000000000000000, -104.6630069175297564 ) ) ;
#3619 = LINE ( 'NONE', #14376, #10626 ) ;
#3620 = EDGE_LOOP ( 'NONE', ( #14113, #13518, #4964, #7899 ) ) ;
#3621 = CARTESIAN_POINT ( 'NONE',  ( 5.039641941650827128, 0.1039572970898357956, -1.141581774561155616 ) ) ;
#3622 = CARTESIAN_POINT ( 'NONE',  ( -3.249999999999999556, 3.250000000000000444, -3.499999999999999556 ) ) ;
#3623 = CARTESIAN_POINT ( 'NONE',  ( -62.68280523391339898, 9.999999999999998224, -198.2448752127049261 ) ) ;
#3624 = CARTESIAN_POINT ( 'NONE',  ( 1.346194077712561166, 5.437500000000000888, -0.2500000000000011102 ) ) ;
#3625 = ORIENTED_EDGE ( 'NONE', *, *, #12319, .T. ) ;
#3626 = CARTESIAN_POINT ( 'NONE',  ( -5.229219651521534118, 9.999999999999998224, -111.7283649857152739 ) ) ;
#3627 = AXIS2_PLACEMENT_3D ( 'NONE', #14889, #12471, #2827 ) ;
#3628 = DIRECTION ( 'NONE',  ( 0.000000000000000000, -0.000000000000000000, 1.000000000000000000 ) ) ;
#3629 = FACE_OUTER_BOUND ( 'NONE', #2549, .T. ) ;
#3630 = ADVANCED_FACE ( 'NONE', ( #13986 ), #6243, .T. ) ;
#3631 = CARTESIAN_POINT ( 'NONE',  ( -3.249999999999999556, 2.250000000000000444, -3.499999999999999556 ) ) ;
#3632 = CARTESIAN_POINT ( 'NONE',  ( 2.651650429449552870, 2.125000000000000000, -6.151650429449553314 ) ) ;
#3633 = CARTESIAN_POINT ( 'NONE',  ( -1.553300858899106407, 5.062500000000000888, 0.2500000000000002220 ) ) ;
#3634 = CARTESIAN_POINT ( 'NONE',  ( -3.025102703132704018, 8.666684749742557836E-31, -116.3639557890653293 ) ) ;
#3635 = CARTESIAN_POINT ( 'NONE',  ( -3.750000000000000000, 7.812500000000000000, -5.053300858899105741 ) ) ;
#3636 = CARTESIAN_POINT ( 'NONE',  ( 0.2814260646950919043, 10.51133653148715652, 2.961392013598888706 ) ) ;
#3637 = CARTESIAN_POINT ( 'NONE',  ( -4.144693943509170531, 10.67450019962763186, -47.43930023633046744 ) ) ;
#3638 = CARTESIAN_POINT ( 'NONE',  ( -8.030143518455577833, 0.4858890952578076017, -104.9565718900056055 ) ) ;
#3639 = CARTESIAN_POINT ( 'NONE',  ( -0.2990415025319886344, 3.999999999999993783, -140.3882592102232820 ) ) ;
#3640 = CARTESIAN_POINT ( 'NONE',  ( 3.249999999999998668, 13.68750000000000000, -4.846194077712560500 ) ) ;
#3641 = DIRECTION ( 'NONE',  ( 0.000000000000000000, -1.000000000000000000, 0.000000000000000000 ) ) ;
#3642 = CARTESIAN_POINT ( 'NONE',  ( -64.92429726018247038, 14.93831521102260496, -187.6311702733107154 ) ) ;
#3643 = ORIENTED_EDGE ( 'NONE', *, *, #1668, .F. ) ;
#3644 = ORIENTED_EDGE ( 'NONE', *, *, #6843, .F. ) ;
#3645 = CARTESIAN_POINT ( 'NONE',  ( -5.948205887739289821, 2.500000000000000444, -109.2829347069437915 ) ) ;
#3646 = CARTESIAN_POINT ( 'NONE',  ( 12.60805090540101681, 8.673617379884035472E-16, -165.7379246688466310 ) ) ;
#3647 = CARTESIAN_POINT ( 'NONE',  ( 3.750000000000000000, 6.750000000000000000, -3.500000000000000444 ) ) ;
#3648 = CARTESIAN_POINT ( 'NONE',  ( 2.651650429449553314, 4.375000000000000000, -0.8483495705504476847 ) ) ;
#3649 = CARTESIAN_POINT ( 'NONE',  ( -18.09353981420590785, 2.305072418039671334, -129.3374956033358671 ) ) ;
#3650 = VERTEX_POINT ( 'NONE', #524 ) ;
#3651 = ADVANCED_FACE ( 'NONE', ( #10182 ), #3168, .F. ) ;
#3652 = CARTESIAN_POINT ( 'NONE',  ( -1.346194077712559167, 3.937500000000000444, -6.749999999999999112 ) ) ;
#3653 = EDGE_CURVE ( 'NONE', #11204, #10207, #12572, .T. ) ;
#3654 = CARTESIAN_POINT ( 'NONE',  ( -69.91247589369663729, 14.99999999999771383, -187.7969989154929351 ) ) ;
#3655 = DIRECTION ( 'NONE',  ( 0.000000000000000000, 0.000000000000000000, 1.000000000000000000 ) ) ;
#3656 = SHAPE_REPRESENTATION_RELATIONSHIP ( 'NONE' , 'NONE' ,  #10891, #5218 ) ;
#3657 = CARTESIAN_POINT ( 'NONE',  ( -3.249999999999999556, 8.187500000000000000, -2.153805922287440833 ) ) ;
#3658 = DIRECTION ( 'NONE',  ( 0.000000000000000000, 1.000000000000000000, 0.000000000000000000 ) ) ;
#3659 = DATE_AND_TIME ( #2739, #990 ) ;
#3660 = CARTESIAN_POINT ( 'NONE',  ( 10.82638304853600530, 14.99999999999719336, -107.3456397789498169 ) ) ;
#3661 = CARTESIAN_POINT ( 'NONE',  ( 9.723706525202544526, 5.000000000000000888, -119.8316069321735284 ) ) ;
#3662 = ORIENTED_EDGE ( 'NONE', *, *, #10486, .F. ) ;
#3663 = CARTESIAN_POINT ( 'NONE',  ( 0.000000000000000000, 0.2105996885190176970, -0.1347136637304948981 ) ) ;
#3664 = CARTESIAN_POINT ( 'NONE',  ( 2.298097038856279362, 13.87500000000000000, -1.201902961143720860 ) ) ;
#3665 = VERTEX_POINT ( 'NONE', #11333 ) ;
#3666 = ORIENTED_EDGE ( 'NONE', *, *, #1065, .F. ) ;
#3667 = LINE ( 'NONE', #10479, #2075 ) ;
#3668 = CARTESIAN_POINT ( 'NONE',  ( 3.749999999999999556, 5.250000000000000000, -3.500000000000000444 ) ) ;
#3669 = CARTESIAN_POINT ( 'NONE',  ( -3.980102097228897738E-16, 8.999999999999998224, -6.749999999999999112 ) ) ;
#3670 = ORIENTED_EDGE ( 'NONE', *, *, #3936, .T. ) ;
#3671 = CARTESIAN_POINT ( 'NONE',  ( 6.491365067585774362, 15.00000000000000000, 0.2705411889128706004 ) ) ;
#3672 = CARTESIAN_POINT ( 'NONE',  ( -1.346194077712559389, 2.437500000000000444, -6.749999999999999112 ) ) ;
#3673 = EDGE_CURVE ( 'NONE', #16, #11237, #1972, .T. ) ;
#3674 = CARTESIAN_POINT ( 'NONE',  ( -6.336334816315998708, 2.500000000000000000, -118.7797536126130353 ) ) ;
#3675 = CARTESIAN_POINT ( 'NONE',  ( 9.044950117654433797, 0.000000000000000000, -137.9826476090360643 ) ) ;
#3676 = COORDINATED_UNIVERSAL_TIME_OFFSET ( 0, 0, .AHEAD. ) ;
#3677 = CARTESIAN_POINT ( 'NONE',  ( -58.04430385666621817, 15.00000000000000355, -164.4058708478957271 ) ) ;
#3678 = ORIENTED_EDGE ( 'NONE', *, *, #13822, .T. ) ;
#3679 = CARTESIAN_POINT ( 'NONE',  ( -10.72138378296757466, 1.921202954650395478, -40.62330995231931041 ) ) ;
#3680 = CARTESIAN_POINT ( 'NONE',  ( -2.651650429449552870, 14.62500000000000178, -0.8483495705504467965 ) ) ;
#3681 = CARTESIAN_POINT ( 'NONE',  ( 30.32986759126112730, 0.7500000000000000000, 45.04214087805580391 ) ) ;
#3682 = CARTESIAN_POINT ( 'NONE',  ( -67.59410015116293380, 10.89016549995086969, -204.3299372489977088 ) ) ;
#3683 = LINE ( 'NONE', #1529, #2767 ) ;
#3684 = CARTESIAN_POINT ( 'NONE',  ( -3.249999999999999112, 3.812500000000000888, -4.846194077712558723 ) ) ;
#3685 = CARTESIAN_POINT ( 'NONE',  ( 10.39131294298060837, 2.427390659499539360, -106.7954589000411829 ) ) ;
#3686 = CALENDAR_DATE ( 2026, 8, 10 ) ;
#3687 = CC_DESIGN_SECURITY_CLASSIFICATION ( #8377, ( #12090 ) ) ;
#3688 = CARTESIAN_POINT ( 'NONE',  ( -32.49979969806455671, 10.00000000000000178, -156.1716796081737186 ) ) ;
#3689 = CARTESIAN_POINT ( 'NONE',  ( 1.041770615072654671, 4.863578055268357403, -139.4526175671829549 ) ) ;
#3690 = CIRCLE ( 'NONE', #9124, 16.00000000006737721 ) ;
#3691 = ORIENTED_EDGE ( 'NONE', *, *, #6476, .F. ) ;
#3692 = CARTESIAN_POINT ( 'NONE',  ( 5.335252549867767868, 0.09849780990753932708, 1.313236408779714814 ) ) ;
#3693 = CARTESIAN_POINT ( 'NONE',  ( -1.346194077712559167, 3.437500000000000000, -6.749999999999999112 ) ) ;
#3694 = CARTESIAN_POINT ( 'NONE',  ( -57.72850238822916680, 10.00000000000000355, -153.7160801922878193 ) ) ;
#3695 = CARTESIAN_POINT ( 'NONE',  ( 0.000000000000000000, 15.00000000000000000, -0.2500000000000002220 ) ) ;
#3696 = CARTESIAN_POINT ( 'NONE',  ( 3.249999999999998224, 5.187500000000001776, -4.846194077712561388 ) ) ;
#3697 = ORIENTED_EDGE ( 'NONE', *, *, #13475, .T. ) ;
#3698 = CARTESIAN_POINT ( 'NONE',  ( -0.1929122761615916781, 15.00000000000000000, -111.6573691072870957 ) ) ;
#3699 = CARTESIAN_POINT ( 'NONE',  ( 0.3014166804839332192, 10.73715447649216514, 2.948015770753482645 ) ) ;
#3700 = APPROVAL_PERSON_ORGANIZATION ( #11475, #3558, #14184 ) ;
#3701 = CARTESIAN_POINT ( 'NONE',  ( 10.43370164639825326, 14.41280555657135309, -106.2140181855886425 ) ) ;
#3702 = CARTESIAN_POINT ( 'NONE',  ( -3.249999999999999556, 0.3125000000000000555, -4.846194077712557835 ) ) ;
#3703 = CARTESIAN_POINT ( 'NONE',  ( 2.651650429449553314, 1.375000000000000000, -0.8483495705504476847 ) ) ;
#3704 = AXIS2_PLACEMENT_3D ( 'NONE', #257, #8439, #9455 ) ;
#3705 = CARTESIAN_POINT ( 'NONE',  ( 0.000000000000000000, 7.000000000000000000, 0.2500000000000002220 ) ) ;
#3706 = CARTESIAN_POINT ( 'NONE',  ( -4.141308399130902984, 10.68732985402159841, -47.42052949952586260 ) ) ;
#3707 = CARTESIAN_POINT ( 'NONE',  ( -3.750000000000000000, 5.812500000000000888, -5.053300858899105741 ) ) ;
#3708 = CARTESIAN_POINT ( 'NONE',  ( 3.398729321283757709, 14.73417332778925015, 0.02313801857711561549 ) ) ;
#3709 = CARTESIAN_POINT ( 'NONE',  ( 9.541413199640935261, 1.119725504013711048E-15, -163.5385917027302867 ) ) ;
#3710 = DIRECTION ( 'NONE',  ( 0.000000000000000000, 0.000000000000000000, 1.000000000000000000 ) ) ;
#3711 = AXIS2_PLACEMENT_3D ( 'NONE', #9906, #11981, #323 ) ;
#3712 = EDGE_CURVE ( 'NONE', #587, #3245, #12580, .T. ) ;
#3713 = CARTESIAN_POINT ( 'NONE',  ( 1.004809442601847236, 6.000000000000000000, -139.4752805618705906 ) ) ;
#3714 = CARTESIAN_POINT ( 'NONE',  ( -3.249999999999999556, 11.25000000000000000, -3.499999999999999556 ) ) ;
#3715 = VECTOR ( 'NONE', #10663, 1000.000000000000000 ) ;
#3716 = AXIS2_PLACEMENT_3D ( 'NONE', #14024, #5742, #7987 ) ;
#3717 = CARTESIAN_POINT ( 'NONE',  ( 7.490632659013988892, 1.449414178213610072, 1.923996036189850267 ) ) ;
#3718 = CARTESIAN_POINT ( 'NONE',  ( -2.524281728693006599, 7.379999999999995453, -45.64919840677852392 ) ) ;
#3719 = AXIS2_PLACEMENT_3D ( 'NONE', #4014, #7556, #12421 ) ;
#3720 = EDGE_LOOP ( 'NONE', ( #15, #12904, #2430, #11906 ) ) ;
#3721 = CARTESIAN_POINT ( 'NONE',  ( 0.000000000000000000, 10.49999999999999822, 0.2500000000000002220 ) ) ;
#3722 = EDGE_LOOP ( 'NONE', ( #7811, #3697, #1894, #7038 ) ) ;
#3723 = CARTESIAN_POINT ( 'NONE',  ( -2.774786199743468629, 4.336808689942017736E-16, -115.4094725772310710 ) ) ;
#3724 = CARTESIAN_POINT ( 'NONE',  ( -21.23553893743079257, 8.673617379884035472E-16, -200.3363993825013836 ) ) ;
#3725 = CARTESIAN_POINT ( 'NONE',  ( -2.651650429449552870, 7.125000000000000000, -0.8483495705504462414 ) ) ;
#3726 = CARTESIAN_POINT ( 'NONE',  ( 1.553300858899109071, 3.437500000000000444, 0.2499999999999989175 ) ) ;
#3727 = LINE ( 'NONE', #8432, #7229 ) ;
#3728 = VERTEX_POINT ( 'NONE', #3140 ) ;
#3729 = CARTESIAN_POINT ( 'NONE',  ( 3.249999999999999556, 4.249999999999999112, -3.500000000000000000 ) ) ;
#3730 = B_SPLINE_CURVE_WITH_KNOTS ( 'NONE', 3,
 ( #9968, #5331, #11427, #6714, #7722, #849, #4177, #12286, #12586, #4255, #6639, #1927, #4329, #1696, #5552, #8882, #8956, #9032 ),
 .UNSPECIFIED., .F., .F.,
 ( 4, 2, 2, 2, 2, 2, 2, 2, 4 ),
 ( 0.000000000000000000, 0.001049529208182857888, 0.002099058416365715777, 0.003148587624548573882, 0.004198116832731431554, 0.005247646040914289225, 0.006297175249097147764, 0.007346704457280005436, 0.008396233665462863108 ),
 .UNSPECIFIED. ) ;
#3731 = VECTOR ( 'NONE', #7643, 1000.000000000000227 ) ;
#3732 = CARTESIAN_POINT ( 'NONE',  ( -61.28061730020114339, 9.999999999999998224, -159.7704501038838885 ) ) ;
#3733 = DIRECTION ( 'NONE',  ( 0.000000000000000000, 1.000000000000000000, 0.000000000000000000 ) ) ;
#3734 = CARTESIAN_POINT ( 'NONE',  ( -2.298097038856278918, 8.375000000000000000, -5.798097038856277585 ) ) ;
#3735 = CARTESIAN_POINT ( 'NONE',  ( -2.546424457856566903, 15.00000000000000711, -122.2590118678561879 ) ) ;
#3736 = CALENDAR_DATE ( 2026, 8, 10 ) ;
#3737 = EDGE_CURVE ( 'NONE', #2801, #6678, #2445, .T. ) ;
#3738 = CARTESIAN_POINT ( 'NONE',  ( -0.6967232357644530527, 6.071532165918824830E-15, -126.1497135265504710 ) ) ;
#3739 = CARTESIAN_POINT ( 'NONE',  ( 11.09126156221322468, 5.000000000000000888, -122.3351348874415123 ) ) ;
#3740 = VERTEX_POINT ( 'NONE', #1677 ) ;
#3741 = ADVANCED_FACE ( 'NONE', ( #9949 ), #4088, .F. ) ;
#3742 = CARTESIAN_POINT ( 'NONE',  ( -2.474470739939843789, 15.00000000000000355, -105.2423196785570525 ) ) ;
#3743 = DIRECTION ( 'NONE',  ( -0.000000000000000000, -1.000000000000000000, -0.000000000000000000 ) ) ;
#3744 = CIRCLE ( 'NONE', #13872, 3.500000000000003109 ) ;
#3745 = ORIENTED_EDGE ( 'NONE', *, *, #7302, .F. ) ;
#3746 = EDGE_LOOP ( 'NONE', ( #13506, #3800, #2390, #8883, #662, #6296 ) ) ;
#3747 = CYLINDRICAL_SURFACE ( 'NONE', #3793, 3.500000000000000000 ) ;
#3748 = CARTESIAN_POINT ( 'NONE',  ( 2.651650429449554203, 6.375000000000000888, -0.8483495705504471296 ) ) ;
#3749 = CARTESIAN_POINT ( 'NONE',  ( 2.298097038856278029, 11.12500000000000000, -5.798097038856279362 ) ) ;
#3750 = ORIENTED_EDGE ( 'NONE', *, *, #15196, .F. ) ;
#3751 = CARTESIAN_POINT ( 'NONE',  ( -5.318033920939080339, 14.99999999999999645, -111.4753907371158306 ) ) ;
#3752 = CARTESIAN_POINT ( 'NONE',  ( -3.249999999999999556, 6.187500000000000888, -2.153805922287440833 ) ) ;
#3753 = PRODUCT_DEFINITION_SHAPE ( 'NONE', 'NONE',  #10001 ) ;
#3754 = APPROVAL_PERSON_ORGANIZATION ( #10341, #4519, #855 ) ;
#3755 = CARTESIAN_POINT ( 'NONE',  ( -5.609104562801103810, 2.500000000000000444, -110.1436424206518296 ) ) ;
#3756 = CARTESIAN_POINT ( 'NONE',  ( 13.13192191588670887, 4.000000000000000000, -166.1703390355876877 ) ) ;
#3757 = PERSON_AND_ORGANIZATION ( #3176, #3020 ) ;
#3758 = EDGE_CURVE ( 'NONE', #15277, #11355, #12338, .T. ) ;
#3759 = CARTESIAN_POINT ( 'NONE',  ( 14.32267195561841611, 15.00000000000000000, -126.6197849905234278 ) ) ;
#3760 = EDGE_CURVE ( 'NONE', #2721, #11588, #3199, .T. ) ;
#3761 = EDGE_CURVE ( 'NONE', #2185, #9168, #3690, .T. ) ;
#3762 = VERTEX_POINT ( 'NONE', #910 ) ;
#3763 = CARTESIAN_POINT ( 'NONE',  ( 1.346194077712560944, 9.937499999999998224, -0.2500000000000010547 ) ) ;
#3764 = CARTESIAN_POINT ( 'NONE',  ( 3.249999999999999556, 13.25000000000000000, -3.500000000000000000 ) ) ;
#3765 = CC_DESIGN_SECURITY_CLASSIFICATION ( #9187, ( #8443 ) ) ;
#3766 = CARTESIAN_POINT ( 'NONE',  ( -0.9087754948914894548, 0.000000000000000000, -45.55632290616385660 ) ) ;
#3767 = CARTESIAN_POINT ( 'NONE',  ( -3.750000000000000000, 14.68750000000000178, -1.946699141100893149 ) ) ;
#3768 = VECTOR ( 'NONE', #5810, 1000.000000000000000 ) ;
#3769 = CARTESIAN_POINT ( 'NONE',  ( -67.62154853663403742, 11.85838142823737407, -203.6530897608368775 ) ) ;
#3770 = CARTESIAN_POINT ( 'NONE',  ( 3.434326385468031368E-15, 9.999999999999998224, -105.0258972447171857 ) ) ;
#3771 = CARTESIAN_POINT ( 'NONE',  ( 3.249999999999999556, 2.249999999999999556, -3.500000000000000000 ) ) ;
#3772 = CARTESIAN_POINT ( 'NONE',  ( 11.03724132942435077, 3.288823991935399871, -106.7036158171736560 ) ) ;
#3773 = PERSON_AND_ORGANIZATION_ROLE ( 'design_owner' ) ;
#3774 = CARTESIAN_POINT ( 'NONE',  ( -1.381864148822929517, 14.99999999999999467, -125.5243971703837502 ) ) ;
#3775 = CARTESIAN_POINT ( 'NONE',  ( -3.648797883638982054, 2.490287375297123962, -1.000000000000000888 ) ) ;
#3776 = ORIENTED_EDGE ( 'NONE', *, *, #2627, .T. ) ;
#3777 = CARTESIAN_POINT ( 'NONE',  ( 6.640721414892046148, 0.6192446679225036554, 3.208961039068100263 ) ) ;
#3778 = CARTESIAN_POINT ( 'NONE',  ( 3.249999999999998668, 5.687500000000000000, -4.846194077712560500 ) ) ;
#3779 = VECTOR ( 'NONE', #1289, 1000.000000000000114 ) ;
#3780 = CARTESIAN_POINT ( 'NONE',  ( -8.808752097635895950, 1.812406719312052994, -105.4646567900641259 ) ) ;
#3781 = CARTESIAN_POINT ( 'NONE',  ( -2.298097038856278918, 13.37500000000000000, -5.798097038856277585 ) ) ;
#3782 = CC_DESIGN_PERSON_AND_ORGANIZATION_ASSIGNMENT ( #4703, #4629, ( #3617 ) ) ;
#3783 = CARTESIAN_POINT ( 'NONE',  ( 3.249999999999998224, 5.312500000000000000, -2.153805922287439945 ) ) ;
#3784 = CARTESIAN_POINT ( 'NONE',  ( -5.170287126225677987, 9.999999999999998224, -112.1835598689908693 ) ) ;
#3785 = FACE_OUTER_BOUND ( 'NONE', #9361, .T. ) ;
#3786 = FACE_OUTER_BOUND ( 'NONE', #13267, .T. ) ;
#3787 = CARTESIAN_POINT ( 'NONE',  ( 0.000000000000000000, 14.50000000000000355, -0.2500000000000002220 ) ) ;
#3788 = CARTESIAN_POINT ( 'NONE',  ( -1.553300858899106407, 6.062500000000000000, 0.2500000000000002220 ) ) ;
#3789 = CARTESIAN_POINT ( 'NONE',  ( 0.03998412334521189021, 2.500000000000000444, 0.4529009045602680472 ) ) ;
#3790 = CARTESIAN_POINT ( 'NONE',  ( -3.749999999999999556, 6.750000000000001776, -3.499999999999999112 ) ) ;
#3791 = AXIS2_PLACEMENT_3D ( 'NONE', #7488, #5326, #7795 ) ;
#3792 = CARTESIAN_POINT ( 'NONE',  ( 3.600783729107427611, 12.34370855950721868, 4.524114163355855034 ) ) ;
#3793 = AXIS2_PLACEMENT_3D ( 'NONE', #2590, #9777, #14509 ) ;
#3794 = CARTESIAN_POINT ( 'NONE',  ( 5.000000000000000888, 9.999999999999998224, -1.663700395152567513 ) ) ;
#3795 = DIRECTION ( 'NONE',  ( 0.9982196940171965682, 0.000000000000000000, -0.05964429961207162734 ) ) ;
#3796 = CARTESIAN_POINT ( 'NONE',  ( 0.1498948966650933412, 8.673617379884034486E-16, -141.0708338584945238 ) ) ;
#3797 = DIRECTION ( 'NONE',  ( 1.000000000000000000, -0.000000000000000000, 0.000000000000000000 ) ) ;
#3798 = CARTESIAN_POINT ( 'NONE',  ( -22.08223501799798782, 8.673617379884035472E-16, -175.4757740284503882 ) ) ;
#3799 = CARTESIAN_POINT ( 'NONE',  ( -64.80993498075393688, 14.11280149795716987, -198.2430571597587630 ) ) ;
#3800 = ORIENTED_EDGE ( 'NONE', *, *, #11404, .T. ) ;
#3801 = CARTESIAN_POINT ( 'NONE',  ( 1.553300858899105963, 11.06250000000000178, -7.250000000000000888 ) ) ;
#3802 = ORIENTED_EDGE ( 'NONE', *, *, #10540, .F. ) ;
#3803 = CARTESIAN_POINT ( 'NONE',  ( -3.700120845809676595, 0.000000000000000000, -118.9498343876333308 ) ) ;
#3804 = CARTESIAN_POINT ( 'NONE',  ( -19.14087761289907874, 8.673617379884035472E-16, -189.8783295055868621 ) ) ;
#3805 = CARTESIAN_POINT ( 'NONE',  ( 3.749999999999999112, 10.81250000000000178, -1.946699141100892039 ) ) ;
#3806 = VECTOR ( 'NONE', #12680, 1000.000000000000000 ) ;
#3807 = CARTESIAN_POINT ( 'NONE',  ( 3.749999999999999556, 9.250000000000001776, -3.500000000000000444 ) ) ;
#3808 = CIRCLE ( 'NONE', #12442, 2.000000000000001776 ) ;
#3809 = CARTESIAN_POINT ( 'NONE',  ( 12.90981819559527111, 1.750000000002257083, 17.95896478634083948 ) ) ;
#3810 = EDGE_LOOP ( 'NONE', ( #13889, #14129, #7978, #9234 ) ) ;
#3811 = CARTESIAN_POINT ( 'NONE',  ( -4.234402844927157794, 4.336808689942017736E-16, -117.4888040839639558 ) ) ;
#3812 = CARTESIAN_POINT ( 'NONE',  ( 0.000000000000000000, 5.500000000000000000, -0.2500000000000002220 ) ) ;
#3813 = CARTESIAN_POINT ( 'NONE',  ( 3.749999999999998668, 8.687500000000000000, -5.053300858899107517 ) ) ;
#3814 = CARTESIAN_POINT ( 'NONE',  ( -69.17701954046839319, 9.999999999999998224, -200.3386666626966246 ) ) ;
#3815 = DIRECTION ( 'NONE',  ( -0.9961255586397050887, 0.000000000000000000, 0.08794243244723005948 ) ) ;
#3816 = SHAPE_REPRESENTATION_RELATIONSHIP ( 'NONE' , 'NONE' ,  #12477, #14249 ) ;
#3817 = CARTESIAN_POINT ( 'NONE',  ( 2.298097038856278473, 7.625000000000000000, -5.798097038856279362 ) ) ;
#3818 = VECTOR ( 'NONE', #876, 1000.000000000000000 ) ;
#3819 = CARTESIAN_POINT ( 'NONE',  ( 19.86183279998939710, 6.000000000000000000, -197.2308909269244168 ) ) ;
#3820 = APPROVAL_ROLE ( '' ) ;
#3821 = CARTESIAN_POINT ( 'NONE',  ( 2.094832066372632084, 4.336808689942017736E-15, -130.8460463719122799 ) ) ;
#3822 = CARTESIAN_POINT ( 'NONE',  ( 6.092154713215619743, 1.734723475976807094E-15, -123.6955108764303048 ) ) ;
#3823 = ORIENTED_EDGE ( 'NONE', *, *, #14188, .F. ) ;
#3824 = DIRECTION ( 'NONE',  ( 0.000000000000000000, 1.000000000000000000, 0.000000000000000000 ) ) ;
#3825 = CARTESIAN_POINT ( 'NONE',  ( -1.346194077712558945, 14.06250000000000178, -0.2500000000000002220 ) ) ;
#3826 = ORIENTED_EDGE ( 'NONE', *, *, #3737, .F. ) ;
#3827 = ORIENTED_EDGE ( 'NONE', *, *, #3372, .F. ) ;
#3828 = CARTESIAN_POINT ( 'NONE',  ( 7.427446726622314976, 7.321094445766561876, -26.41501464507892294 ) ) ;
#3829 = CARTESIAN_POINT ( 'NONE',  ( -2.651650429449552870, 10.87500000000000000, -6.151650429449552426 ) ) ;
#3830 = CARTESIAN_POINT ( 'NONE',  ( -1.346194077712558945, 7.562500000000000888, -0.2500000000000002220 ) ) ;
#3831 = CARTESIAN_POINT ( 'NONE',  ( -3.249999999999999556, 8.750000000000000000, -3.500000000000000000 ) ) ;
#3832 = ADVANCED_FACE ( 'NONE', ( #3442 ), #11966, .T. ) ;
#3833 = ORIENTED_EDGE ( 'NONE', *, *, #2995, .T. ) ;
#3834 = CARTESIAN_POINT ( 'NONE',  ( -7.070709739118031578, 8.673617379884037444E-16, -176.2010769231267489 ) ) ;
#3835 = CARTESIAN_POINT ( 'NONE',  ( -3.249999999999999556, 5.312500000000001776, -4.846194077712557835 ) ) ;
#3836 = EDGE_CURVE ( 'NONE', #1255, #5136, #10628, .T. ) ;
#3837 = CARTESIAN_POINT ( 'NONE',  ( -24.62038850795502043, 3.897326768351937698, -208.8858515350064806 ) ) ;
#3838 = CARTESIAN_POINT ( 'NONE',  ( -55.37984062407457486, 9.999999999999998224, -173.4719643169354413 ) ) ;
#3839 = DIRECTION ( 'NONE',  ( 0.000000000000000000, 0.000000000000000000, 1.000000000000000000 ) ) ;
#3840 = PERSON_AND_ORGANIZATION ( #3176, #3020 ) ;
#3841 = FACE_OUTER_BOUND ( 'NONE', #6749, .T. ) ;
#3842 = B_SPLINE_CURVE_WITH_KNOTS ( 'NONE', 3,
 ( #5083, #2684, #9796, #3925, #13360, #12186, #1606, #5158, #12413, #8006, #11257, #1910, #15061, #752, #11411, #14985, #4310, #15140, #10408, #829 ),
 .UNSPECIFIED., .F., .F.,
 ( 4, 2, 2, 2, 2, 2, 2, 2, 2, 4 ),
 ( 0.000000000000000000, 0.005303151365135050539, 0.01060630273027009934, 0.02121260546054020216, 0.03181890819081030497, 0.04242521092108039737, 0.05303151365135049672, 0.06363781638162059606, 0.07424411911189068847, 0.08485042184216079475 ),
 .UNSPECIFIED. ) ;
#3843 = ORIENTED_EDGE ( 'NONE', *, *, #1110, .T. ) ;
#3844 = CARTESIAN_POINT ( 'NONE',  ( 2.298097038856278473, 0.6250000000000000000, -5.798097038856279362 ) ) ;
#3845 = CARTESIAN_POINT ( 'NONE',  ( 1.553300858899108849, 13.93750000000000000, 0.2499999999999993616 ) ) ;
#3846 = CARTESIAN_POINT ( 'NONE',  ( 10.97171279554003043, 8.773889247172311556, -44.61149169061435060 ) ) ;
#3847 = EDGE_CURVE ( 'NONE', #2992, #4833, #3916, .T. ) ;
#3848 = CARTESIAN_POINT ( 'NONE',  ( -3.749999999999999556, 11.75000000000000178, -3.499999999999999112 ) ) ;
#3849 = EDGE_CURVE ( 'NONE', #6985, #11984, #1543, .T. ) ;
#3850 = EDGE_CURVE ( 'NONE', #5223, #11706, #11482, .T. ) ;
#3851 = CARTESIAN_POINT ( 'NONE',  ( -67.63542228451777305, 12.84083462875344317, -202.2854057673654324 ) ) ;
#3852 = DIRECTION ( 'NONE',  ( 0.000000000000000000, -1.000000000000000000, 0.000000000000000000 ) ) ;
#3853 = CARTESIAN_POINT ( 'NONE',  ( 3.249999999999999556, 1.250000000000000222, -3.500000000000000000 ) ) ;
#3854 = CARTESIAN_POINT ( 'NONE',  ( 6.612393103706271091, -6.831570436677307681E-13, -105.0937218669710944 ) ) ;
#3855 = PERSON_AND_ORGANIZATION ( #3176, #3020 ) ;
#3856 = DIRECTION ( 'NONE',  ( 0.000000000000000000, -0.000000000000000000, 1.000000000000000000 ) ) ;
#3857 = DIRECTION ( 'NONE',  ( 0.000000000000000000, 0.000000000000000000, -1.000000000000000000 ) ) ;
#3858 = ORIENTED_EDGE ( 'NONE', *, *, #10627, .F. ) ;
#3859 = CARTESIAN_POINT ( 'NONE',  ( 4.697001853051453679, 0.007744268132012307668, -0.2236376289218673930 ) ) ;
#3860 = CARTESIAN_POINT ( 'NONE',  ( 2.298097038856278473, 6.625000000000000000, -5.798097038856279362 ) ) ;
#3861 = CARTESIAN_POINT ( 'NONE',  ( -56.93003040406973270, 9.999999999999998224, -152.4998193340993282 ) ) ;
#3862 = CARTESIAN_POINT ( 'NONE',  ( -3.249999999999999112, 0.8124999999999997780, -4.846194077712558723 ) ) ;
#3863 = CARTESIAN_POINT ( 'NONE',  ( 2.298097038856279362, 10.37500000000000000, -1.201902961143720860 ) ) ;
#3864 = DIRECTION ( 'NONE',  ( 0.000000000000000000, 0.000000000000000000, 1.000000000000000000 ) ) ;
#3865 = CARTESIAN_POINT ( 'NONE',  ( 2.786934050261072215, 14.45009198851748522, 0.8495871595598972759 ) ) ;
#3866 = CARTESIAN_POINT ( 'NONE',  ( 9.846296305695277695, 14.78380347570996456, -106.2491606183390047 ) ) ;
#3867 = CARTESIAN_POINT ( 'NONE',  ( -1.346194077712559389, 4.437500000000000888, -6.749999999999999112 ) ) ;
#3868 = CARTESIAN_POINT ( 'NONE',  ( -2.298097038856279362, 14.87500000000000355, -5.798097038856278473 ) ) ;
#3869 = EDGE_CURVE ( 'NONE', #5891, #7451, #4758, .T. ) ;
#3870 = CARTESIAN_POINT ( 'NONE',  ( -1.553300858899107073, 6.437500000000000888, -7.250000000000000000 ) ) ;
#3871 = CARTESIAN_POINT ( 'NONE',  ( -4.100181976537629502, 10.82147003695433796, -47.20166826208706823 ) ) ;
#3872 = CARTESIAN_POINT ( 'NONE',  ( -1.553300858899106629, 5.562500000000001776, 0.2500000000000002220 ) ) ;
#3873 = CARTESIAN_POINT ( 'NONE',  ( 2.648785598488645476, 14.36106363934144703, 0.9962225538062225993 ) ) ;
#3874 = CARTESIAN_POINT ( 'NONE',  ( 10.53129000145030325, 0.3802680776936400719, -164.5383768468789754 ) ) ;
#3875 = DIRECTION ( 'NONE',  ( -0.1564344650402312298, -0.000000000000000000, 0.9876883405951376593 ) ) ;
#3876 = CARTESIAN_POINT ( 'NONE',  ( 0.000000000000000000, 11.00000000000000000, -0.2500000000000002220 ) ) ;
#3877 = CARTESIAN_POINT ( 'NONE',  ( 28.48375933933716198, 5.321094445766561876, -22.19653139158566901 ) ) ;
#3878 = CARTESIAN_POINT ( 'NONE',  ( 6.222862683364174252, 0.008970098793881749535, -139.3955611241877079 ) ) ;
#3879 = CARTESIAN_POINT ( 'NONE',  ( 6.268325292624917999, 0.5457983033243376525, 0.8953897332030867906 ) ) ;
#3880 = LINE ( 'NONE', #10394, #11594 ) ;
#3881 = ORIENTED_EDGE ( 'NONE', *, *, #1683, .T. ) ;
#3882 = PRODUCT_DEFINITION_SHAPE ( 'NONE', 'NONE',  #8872 ) ;
#3883 = CARTESIAN_POINT ( 'NONE',  ( 3.749999999999999112, 11.18750000000000178, -5.053300858899108405 ) ) ;
#3884 = ORIENTED_EDGE ( 'NONE', *, *, #12073, .F. ) ;
#3885 = CARTESIAN_POINT ( 'NONE',  ( -5.689254932628163175, -1.854186021507445874E-12, -117.0567294046643099 ) ) ;
#3886 = CARTESIAN_POINT ( 'NONE',  ( 9.068716941525991615, 0.000000000000000000, -163.1923081219560174 ) ) ;
#3887 = CARTESIAN_POINT ( 'NONE',  ( 3.749999999999998668, 7.687500000000000000, -5.053300858899107517 ) ) ;
#3888 = CARTESIAN_POINT ( 'NONE',  ( -2.651650429449552870, 9.875000000000000000, -6.151650429449552426 ) ) ;
#3889 = DIRECTION ( 'NONE',  ( 1.000000000000000000, 0.000000000000000000, 0.000000000000000000 ) ) ;
#3890 = ORIENTED_EDGE ( 'NONE', *, *, #11293, .T. ) ;
#3891 = CARTESIAN_POINT ( 'NONE',  ( -1.346194077712558945, 2.562500000000000444, -0.2500000000000002220 ) ) ;
#3892 = CARTESIAN_POINT ( 'NONE',  ( 1.553300858899108849, 10.93750000000000000, 0.2499999999999993616 ) ) ;
#3893 = CLOSED_SHELL ( 'NONE', ( #5157, #6080, #1131, #5408, #6126, #5635 ) ) ;
#3894 = CARTESIAN_POINT ( 'NONE',  ( -56.84718378481262135, 15.00000000000000000, -162.0882091452447185 ) ) ;
#3895 = FACE_OUTER_BOUND ( 'NONE', #11410, .T. ) ;
#3896 = DIRECTION ( 'NONE',  ( 1.000000000000000000, 0.000000000000000000, 0.000000000000000000 ) ) ;
#3897 = CARTESIAN_POINT ( 'NONE',  ( 2.298097038856278473, 8.625000000000000000, -5.798097038856279362 ) ) ;
#3898 = DIRECTION ( 'NONE',  ( 1.076984184057326235E-17, 1.000000000000000000, 1.219901976936983860E-16 ) ) ;
#3899 = ITEM_DEFINED_TRANSFORMATION ( 'NONE', 'NONE', #5721,  #9419 ) ;
#3900 = CARTESIAN_POINT ( 'NONE',  ( -1.898078448822344777, -8.673617379884035472E-16, -123.6789374535451316 ) ) ;
#3901 = DIRECTION ( 'NONE',  ( -0.7575874476598363216, 0.000000000000000000, -0.6527336816407245390 ) ) ;
#3902 = ORIENTED_EDGE ( 'NONE', *, *, #9597, .T. ) ;
#3903 = LINE ( 'NONE', #1653, #5689 ) ;
#3904 = CARTESIAN_POINT ( 'NONE',  ( 10.98449875134631348, 11.68766637954128029, -45.34906074712609581 ) ) ;
#3905 = ORIENTED_EDGE ( 'NONE', *, *, #8058, .T. ) ;
#3906 = B_SPLINE_CURVE_WITH_KNOTS ( 'NONE', 3,
 ( #36, #9308, #14110, #8219, #3428, #1268, #11771, #12869, #2281, #5973, #6987, #112, #1190, #5892, #4747, #9538, #14264, #8364, #13095, #2509, #11626, #188, #4898, #14339, #3742, #1044, #2664, #9846 ),
 .UNSPECIFIED., .F., .F.,
 ( 4, 2, 2, 2, 2, 2, 2, 2, 2, 2, 2, 2, 2, 4 ),
 ( 1.734723475976807094E-18, 0.003819759381942296628, 0.007639518763884591522, 0.01145927814582688685, 0.01336915783679803495, 0.01527903752776918131, 0.01718891721874032941, 0.01909879690971147403, 0.02291855629165377023, 0.02387349613713933560, 0.02482843598262490098, 0.02673831567359602479, 0.02864819536456715554, 0.03055807505553827935 ),
 .UNSPECIFIED. ) ;
#3907 = ORIENTED_EDGE ( 'NONE', *, *, #1491, .T. ) ;
#3908 = DIRECTION ( 'NONE',  ( 0.9961255586397050887, -0.000000000000000000, -0.08794243244723005948 ) ) ;
#3909 =( BOUNDED_SURFACE ( )  B_SPLINE_SURFACE ( 3, 2, ( 
 ( #7167, #6092, #12989 ),
 ( #8332, #5862, #11970 ),
 ( #2471, #223, #2552 ),
 ( #1390, #152, #9741 ),
 ( #11888, #14228, #7330 ),
 ( #14301, #5023, #10662 ),
 ( #10808, #11811, #1311 ),
 ( #8410, #10581, #9573 ),
 ( #3957, #7252, #4790 ),
 ( #5939, #4939, #7090 ) ),
 .UNSPECIFIED., .F., .F., .T. ) 
 B_SPLINE_SURFACE_WITH_KNOTS ( ( 4, 2, 2, 2, 4 ),
 ( 3, 3 ),
 ( -2.081668171172168513E-17, 0.009142429936519532591, 0.01828485987303908600, 0.02742728980955863941, 0.03656971974607819281 ),
 ( 0.000000000000000000, 1.000000000000000000 ),
 .UNSPECIFIED. ) 
 GEOMETRIC_REPRESENTATION_ITEM ( )  RATIONAL_B_SPLINE_SURFACE ( (
 ( 1.000000000000000000, 0.7071067811865475727, 1.000000000000000000),
 ( 1.000000000000000000, 0.7071067811865475727, 1.000000000000000000),
 ( 1.000000000000000000, 0.7071067811865475727, 1.000000000000000000),
 ( 1.000000000000000000, 0.7071067811865475727, 1.000000000000000000),
 ( 1.000000000000000000, 0.7071067811865475727, 1.000000000000000000),
 ( 1.000000000000000000, 0.7071067811865475727, 1.000000000000000000),
 ( 1.000000000000000000, 0.7071067811865475727, 1.000000000000000000),
 ( 1.000000000000000000, 0.7071067811865475727, 1.000000000000000000),
 ( 1.000000000000000000, 0.7071067811865475727, 1.000000000000000000),
 ( 1.000000000000000000, 0.7071067811865475727, 1.000000000000000000) ) ) 
 REPRESENTATION_ITEM ( '' )  SURFACE ( )  );
#3910 = CARTESIAN_POINT ( 'NONE',  ( -1.553300858899106629, 12.56250000000000355, 0.2499999999999998335 ) ) ;
#3911 = CARTESIAN_POINT ( 'NONE',  ( -2.298097038856279362, 10.87500000000000000, -5.798097038856278473 ) ) ;
#3912 = CARTESIAN_POINT ( 'NONE',  ( -1.346194077712559167, 11.93750000000000178, -6.749999999999999112 ) ) ;
#3913 = ORIENTED_EDGE ( 'NONE', *, *, #9574, .T. ) ;
#3914 = CARTESIAN_POINT ( 'NONE',  ( -1.586855474368330077, 14.99999999999999822, -114.8059160835097714 ) ) ;
#3915 = CARTESIAN_POINT ( 'NONE',  ( 0.000000000000000000, 8.000000000000000000, -0.2500000000000002220 ) ) ;
#3916 = LINE ( 'NONE', #4836, #15071 ) ;
#3917 = CARTESIAN_POINT ( 'NONE',  ( 4.083862360612559250, 0.1767556829816783193, -0.01992505507647806748 ) ) ;
#3918 = CARTESIAN_POINT ( 'NONE',  ( -62.18589641907635013, 15.00000000000000178, -176.3558874768298210 ) ) ;
#3919 = PERSON_AND_ORGANIZATION ( #3176, #3020 ) ;
#3920 = CARTESIAN_POINT ( 'NONE',  ( -9.240119717576689595, 2.500000000000000444, -104.6630069175297564 ) ) ;
#3921 = ORIENTED_EDGE ( 'NONE', *, *, #2993, .T. ) ;
#3922 = EDGE_CURVE ( 'NONE', #4505, #4915, #2522, .T. ) ;
#3923 = CARTESIAN_POINT ( 'NONE',  ( 3.249999999999998224, 14.18750000000000178, -4.846194077712561388 ) ) ;
#3924 = CARTESIAN_POINT ( 'NONE',  ( 3.749999999999998668, 11.68750000000000000, -5.053300858899107517 ) ) ;
#3925 = CARTESIAN_POINT ( 'NONE',  ( -4.261429542763926825, 1.750000000000027756, 3.010279858880415826 ) ) ;
#3926 = CARTESIAN_POINT ( 'NONE',  ( 3.750000000000000000, 1.750000000000000000, -3.500000000000000444 ) ) ;
#3927 = CARTESIAN_POINT ( 'NONE',  ( -63.33207902479660589, 11.17285071206491409, -203.3434558358833328 ) ) ;
#3928 = CARTESIAN_POINT ( 'NONE',  ( 4.286263797015736595E-16, 5.000000000000000000, 3.500000000000000000 ) ) ;
#3929 = CARTESIAN_POINT ( 'NONE',  ( 11.32911568800036761, 5.000000000000000888, -106.8195553349435301 ) ) ;
#3930 = DATE_TIME_ROLE ( 'creation_date' ) ;
#3931 = CARTESIAN_POINT ( 'NONE',  ( -9.030574454602197321, 2.490287375297123518, -34.97919997656152447 ) ) ;
#3932 = CARTESIAN_POINT ( 'NONE',  ( 11.04730217088347644, 12.49999999999999822, -107.1178495010082656 ) ) ;
#3933 = ORIENTED_EDGE ( 'NONE', *, *, #4138, .T. ) ;
#3934 = CARTESIAN_POINT ( 'NONE',  ( 5.625964192004158981, 0.1718480277638484433, 1.809263816539721015 ) ) ;
#3935 = CARTESIAN_POINT ( 'NONE',  ( -1.346194077712559167, 7.437500000000000888, -6.749999999999999112 ) ) ;
#3936 = EDGE_CURVE ( 'NONE', #8666, #6652, #5224, .T. ) ;
#3937 = CARTESIAN_POINT ( 'NONE',  ( -8.512683829985039807, 0.7114776304792922446, -104.8579508657064849 ) ) ;
#3938 = CARTESIAN_POINT ( 'NONE',  ( 3.249999999999999556, 12.75000000000000178, -3.500000000000000000 ) ) ;
#3939 = CARTESIAN_POINT ( 'NONE',  ( -3.980102097228897738E-16, 10.00000000000000000, -6.749999999999999112 ) ) ;
#3940 = CARTESIAN_POINT ( 'NONE',  ( -3.850191409010146781, 7.379999999999995453, -49.29672681923015887 ) ) ;
#3941 = CARTESIAN_POINT ( 'NONE',  ( -1.346194077712559389, 0.4375000000000000555, -6.749999999999999112 ) ) ;
#3942 = CARTESIAN_POINT ( 'NONE',  ( -0.4453226528549816265, -2.225540348348185052E-17, -1.000000000000000000 ) ) ;
#3943 = CARTESIAN_POINT ( 'NONE',  ( -3.249999999999999556, 3.250000000000000444, -3.499999999999999556 ) ) ;
#3944 = CARTESIAN_POINT ( 'NONE',  ( -3.249999999999999556, 14.75000000000000000, -3.500000000000000000 ) ) ;
#3945 = CARTESIAN_POINT ( 'NONE',  ( -1.553300858899107073, 10.43750000000000000, -7.250000000000000000 ) ) ;
#3946 = CC_DESIGN_APPROVAL ( #4078, ( #10487 ) ) ;
#3947 = CARTESIAN_POINT ( 'NONE',  ( 0.2510614944550047523, 4.187370637758943026, 2.843778190552137985 ) ) ;
#3948 = CARTESIAN_POINT ( 'NONE',  ( 0.000000000000000000, 7.500000000000000888, 0.2500000000000002220 ) ) ;
#3949 = CARTESIAN_POINT ( 'NONE',  ( 4.831928030476276170, 14.67058913578727264, 0.7643627623969961871 ) ) ;
#3950 = AXIS2_PLACEMENT_3D ( 'NONE', #3982, #11305, #726 ) ;
#3951 = CARTESIAN_POINT ( 'NONE',  ( -5.488578029460351893, -2.075239479414269894, -43.69424231201529096 ) ) ;
#3952 = CARTESIAN_POINT ( 'NONE',  ( 1.114947364559086829, 6.000000000000000000, -139.4079432275550232 ) ) ;
#3953 = CARTESIAN_POINT ( 'NONE',  ( 26.58801926426209405, 6.000000000000000000, -139.0072983920785532 ) ) ;
#3954 = ADVANCED_FACE ( 'NONE', ( #4219 ), #5914, .T. ) ;
#3955 = CARTESIAN_POINT ( 'NONE',  ( -9.695200183287226992, 8.673617379884037444E-16, -155.2279384737427108 ) ) ;
#3956 = ORIENTED_EDGE ( 'NONE', *, *, #12449, .F. ) ;
#3957 = CARTESIAN_POINT ( 'NONE',  ( -14.37903708472870790, 9.999999999999998224, -152.3617959901736754 ) ) ;
#3958 = CARTESIAN_POINT ( 'NONE',  ( 2.651650429449552870, 13.12499999999999822, -6.151650429449555091 ) ) ;
#3959 = ORIENTED_EDGE ( 'NONE', *, *, #11381, .T. ) ;
#3960 = CARTESIAN_POINT ( 'NONE',  ( 0.000000000000000000, 3.061616997868383018E-17, 0.2500000000000002220 ) ) ;
#3961 = VECTOR ( 'NONE', #570, 1000.000000000000000 ) ;
#3962 = CARTESIAN_POINT ( 'NONE',  ( -12.21562406281302415, 3.999999999997721378, -189.0327199747631255 ) ) ;
#3963 = CARTESIAN_POINT ( 'NONE',  ( 0.000000000000000000, 10.00000000000000000, 0.2500000000000002220 ) ) ;
#3964 = CARTESIAN_POINT ( 'NONE',  ( 1.553300858899109071, 9.437500000000003553, 0.2499999999999989175 ) ) ;
#3965 = AXIS2_PLACEMENT_3D ( 'NONE', #10687, #105, #3655 ) ;
#3966 = CARTESIAN_POINT ( 'NONE',  ( 3.158384440324536691, 0.000000000000000000, -1.000000000000001332 ) ) ;
#3967 = EDGE_LOOP ( 'NONE', ( #9214, #2902, #7394, #7372, #7939, #7158, #10529, #10261, #4608, #325, #10881, #13998 ) ) ;
#3968 = CARTESIAN_POINT ( 'NONE',  ( -2.298097038856278029, 5.625000000000000000, -1.201902961143720638 ) ) ;
#3969 = CARTESIAN_POINT ( 'NONE',  ( 3.750000000000000000, 11.75000000000000000, -3.500000000000000444 ) ) ;
#3970 = CARTESIAN_POINT ( 'NONE',  ( -64.95288741863723203, 15.00000000000000000, -195.5112306306130563 ) ) ;
#3971 = SECURITY_CLASSIFICATION ( '', '', #15047 ) ;
#3972 = CARTESIAN_POINT ( 'NONE',  ( 26.17093350124942219, 5.000000000000000888, -137.7213801722282653 ) ) ;
#3973 = PERSON_AND_ORGANIZATION ( #3176, #3020 ) ;
#3974 = CARTESIAN_POINT ( 'NONE',  ( 3.249999999999999556, 9.750000000000000000, -3.500000000000000000 ) ) ;
#3975 = AXIS2_PLACEMENT_3D ( 'NONE', #1777, #7642, #13757 ) ;
#3976 = CARTESIAN_POINT ( 'NONE',  ( -0.9552437115555381109, 15.00000000000000711, -125.6272940116446364 ) ) ;
#3977 = VECTOR ( 'NONE', #457, 1000.000000000000000 ) ;
#3978 = CARTESIAN_POINT ( 'NONE',  ( -4.665009673976214799, 5.000000000003948841, -129.3402154207116155 ) ) ;
#3979 = CARTESIAN_POINT ( 'NONE',  ( 3.294401254219998965, 1.734723475976807094E-15, -113.2772910607207848 ) ) ;
#3980 = ORIENTED_EDGE ( 'NONE', *, *, #5073, .T. ) ;
#3981 = DIRECTION ( 'NONE',  ( -0.02181900108494707127, 0.000000000000000000, 0.9997619372588930631 ) ) ;
#3982 = CARTESIAN_POINT ( 'NONE',  ( 6.369258321017759350, -2.075239479414269894, -34.56909192082981974 ) ) ;
#3983 = EDGE_LOOP ( 'NONE', ( #7268, #12003, #3377, #1267 ) ) ;
#3984 = CARTESIAN_POINT ( 'NONE',  ( -0.2500000000000000555, 4.500000000000000888, 1.500000000000000222 ) ) ;
#3985 = CARTESIAN_POINT ( 'NONE',  ( 0.2508815455408998085, 0.2972145640522015908, -6.863050255469942407 ) ) ;
#3986 = CARTESIAN_POINT ( 'NONE',  ( -3.750000000000000000, 13.81250000000000178, -5.053300858899105741 ) ) ;
#3987 = CARTESIAN_POINT ( 'NONE',  ( 1.346194077712558279, 12.06250000000000000, -6.750000000000000888 ) ) ;
#3988 = CARTESIAN_POINT ( 'NONE',  ( -2.298097038856278029, 10.62500000000000000, -1.201902961143720638 ) ) ;
#3989 = ORIENTED_EDGE ( 'NONE', *, *, #7231, .T. ) ;
#3990 = AXIS2_PLACEMENT_3D ( 'NONE', #14239, #3641, #3339 ) ;
#3991 = CARTESIAN_POINT ( 'NONE',  ( -67.58382170693634805, 5.000000000000000000, -204.5178482451963191 ) ) ;
#3992 = AXIS2_PLACEMENT_3D ( 'NONE', #15011, #11515, #8891 ) ;
#3993 = CARTESIAN_POINT ( 'NONE',  ( 2.298097038856279362, 8.875000000000001776, -1.201902961143720860 ) ) ;
#3994 = VECTOR ( 'NONE', #8269, 1000.000000000000000 ) ;
#3995 = CARTESIAN_POINT ( 'NONE',  ( 0.000000000000000000, 9.999999999999998224, -100.6237003951525679 ) ) ;
#3996 = CARTESIAN_POINT ( 'NONE',  ( 13.21422700454708909, 13.96506978500478802, -126.0492241132350415 ) ) ;
#3997 = FACE_OUTER_BOUND ( 'NONE', #5565, .T. ) ;
#3998 = CARTESIAN_POINT ( 'NONE',  ( -52.62960184830343735, 14.99999999999999822, -160.4142894912321822 ) ) ;
#3999 = CALENDAR_DATE ( 2026, 8, 10 ) ;
#4000 = AXIS2_PLACEMENT_3D ( 'NONE', #4274, #5499, #4196 ) ;
#4001 = CARTESIAN_POINT ( 'NONE',  ( -14.68073284315481253, 7.499999999999991118, -92.37694453701993780 ) ) ;
#4002 = EDGE_LOOP ( 'NONE', ( #7512, #4853, #14242, #10312 ) ) ;
#4003 = CARTESIAN_POINT ( 'NONE',  ( 1.346194077712560944, 1.937500000000000000, -0.2500000000000010547 ) ) ;
#4004 = CARTESIAN_POINT ( 'NONE',  ( 1.553300858899108849, 14.93750000000000178, 0.2499999999999993616 ) ) ;
#4005 = ORIENTED_EDGE ( 'NONE', *, *, #12260, .F. ) ;
#4006 = DIRECTION ( 'NONE',  ( 0.000000000000000000, 0.000000000000000000, 1.000000000000000000 ) ) ;
#4007 = AXIS2_PLACEMENT_3D ( 'NONE', #1898, #2906, #1823 ) ;
#4008 = CARTESIAN_POINT ( 'NONE',  ( 3.749999999999999112, 2.812500000000000000, -1.946699141100892039 ) ) ;
#4009 = CARTESIAN_POINT ( 'NONE',  ( -63.21422130130007133, 5.000000000000000888, -203.6040552426024988 ) ) ;
#4010 = DIRECTION ( 'NONE',  ( 0.000000000000000000, -1.000000000000000000, 0.000000000000000000 ) ) ;
#4011 = CARTESIAN_POINT ( 'NONE',  ( -2.651650429449552870, 1.125000000000000222, -0.8483495705504462414 ) ) ;
#4012 = APPROVAL_ROLE ( '' ) ;
#4013 = CARTESIAN_POINT ( 'NONE',  ( -67.63558047453210520, 12.45480787954772062, -202.9260935043153324 ) ) ;
#4014 = CARTESIAN_POINT ( 'NONE',  ( 9.971950858281140029, 8.773889247172311556, -44.63331069169930032 ) ) ;
#4015 = APPROVAL_PERSON_ORGANIZATION ( #455, #6528, #14374 ) ;
#4016 = ORIENTED_EDGE ( 'NONE', *, *, #2625, .T. ) ;
#4017 = CARTESIAN_POINT ( 'NONE',  ( -3.980102097228897245E-16, 8.500000000000000000, -6.749999999999999112 ) ) ;
#4018 = CARTESIAN_POINT ( 'NONE',  ( -8.763338091613618985, 1.650112951118430704, -105.4343884788352455 ) ) ;
#4019 = CARTESIAN_POINT ( 'NONE',  ( -1.346194077712559389, 12.06250000000000000, -0.2500000000000002220 ) ) ;
#4020 = CARTESIAN_POINT ( 'NONE',  ( -3.249999999999999112, 8.812500000000001776, -4.846194077712558723 ) ) ;
#4021 = CARTESIAN_POINT ( 'NONE',  ( 4.544676675852343806, 6.000000000000000000, -126.1782412829290934 ) ) ;
#4022 = FACE_OUTER_BOUND ( 'NONE', #2043, .T. ) ;
#4023 = CARTESIAN_POINT ( 'NONE',  ( 10.62587365868640710, 14.24122074427556583, -106.5450489676481283 ) ) ;
#4024 = CARTESIAN_POINT ( 'NONE',  ( -3.249999999999999556, 4.250000000000000000, -3.499999999999999556 ) ) ;
#4025 = CARTESIAN_POINT ( 'NONE',  ( 2.651650429449553314, 7.375000000000000000, -0.8483495705504476847 ) ) ;
#4026 = CARTESIAN_POINT ( 'NONE',  ( 0.000000000000000000, 9.000000000000001776, 0.2500000000000002220 ) ) ;
#4027 = EDGE_CURVE ( 'NONE', #6914, #9763, #10384, .T. ) ;
#4028 = CARTESIAN_POINT ( 'NONE',  ( 8.475206276408092876, 0.000000000000000000, -34.56909192082981974 ) ) ;
#4029 = CARTESIAN_POINT ( 'NONE',  ( -3.482786547411536038, 10.52217399014809729, -46.42572704807074047 ) ) ;
#4030 = CARTESIAN_POINT ( 'NONE',  ( 2.651650429449552870, 11.12500000000000000, -6.151650429449555091 ) ) ;
#4031 = CARTESIAN_POINT ( 'NONE',  ( 9.939878312292615092, 9.999999999999998224, -115.2320631035898373 ) ) ;
#4032 = CARTESIAN_POINT ( 'NONE',  ( 12.77611550990255829, 4.050274393866083678, -166.6173057128717687 ) ) ;
#4033 = AXIS2_PLACEMENT_3D ( 'NONE', #14761, #10954, #2766 ) ;
#4034 = CARTESIAN_POINT ( 'NONE',  ( 30.66256791564903139, 2.100000000000000089, 35.19913216203716644 ) ) ;
#4035 = CARTESIAN_POINT ( 'NONE',  ( -30.46290170330349056, 4.000000000000174971, -196.8214803422608270 ) ) ;
#4036 = CARTESIAN_POINT ( 'NONE',  ( -8.289881740238502772, 2.075239479414269894, -35.21986562831451550 ) ) ;
#4037 = CARTESIAN_POINT ( 'NONE',  ( 8.894904190497955554, 4.261448547226525996, 2.831834529235428999 ) ) ;
#4038 = CARTESIAN_POINT ( 'NONE',  ( -1.553300858899107073, 11.93750000000000178, -7.249999999999999112 ) ) ;
#4039 = ORIENTED_EDGE ( 'NONE', *, *, #13822, .F. ) ;
#4040 = CARTESIAN_POINT ( 'NONE',  ( 10.32040002734022188, 15.00000000000000000, -106.4311084481271763 ) ) ;
#4041 = CARTESIAN_POINT ( 'NONE',  ( -20.62911563925012359, 8.673617379884035472E-16, -191.9171239689855781 ) ) ;
#4042 = CARTESIAN_POINT ( 'NONE',  ( -2.651650429449553314, 7.375000000000000888, -6.151650429449552426 ) ) ;
#4043 = CARTESIAN_POINT ( 'NONE',  ( -4.592425496802573972E-16, 10.00000000000000000, -7.250000000000000000 ) ) ;
#4044 = CARTESIAN_POINT ( 'NONE',  ( -65.53364736412717662, 15.00000000000000000, -203.4171941195418754 ) ) ;
#4045 = ORIENTED_EDGE ( 'NONE', *, *, #13279, .T. ) ;
#4046 = VECTOR ( 'NONE', #1485, 1000.000000000000000 ) ;
#4047 = CARTESIAN_POINT ( 'NONE',  ( -3.249999999999999112, 6.812500000000000000, -4.846194077712558723 ) ) ;
#4048 = CIRCLE ( 'NONE', #100, 2.000000000000001776 ) ;
#4049 = ADVANCED_FACE ( 'NONE', ( #8613, #13349 ), #11022, .F. ) ;
#4050 = CARTESIAN_POINT ( 'NONE',  ( 1.553300858899108849, 8.937500000000001776, 0.2499999999999993616 ) ) ;
#4051 = B_SPLINE_CURVE_WITH_KNOTS ( 'NONE', 3,
 ( #4479, #15239, #1077, #9188, #8028, #9342 ),
 .UNSPECIFIED., .F., .F.,
 ( 4, 2, 4 ),
 ( 1.398578778534940505E-17, 0.001339092541177541208, 0.002678185082355068539 ),
 .UNSPECIFIED. ) ;
#4052 = CARTESIAN_POINT ( 'NONE',  ( -68.82095148151569219, 14.99999999999884359, -201.5743162692542398 ) ) ;
#4053 = EDGE_CURVE ( 'NONE', #3728, #16, #12965, .T. ) ;
#4054 = EDGE_CURVE ( 'NONE', #9168, #8798, #4661, .T. ) ;
#4055 = CARTESIAN_POINT ( 'NONE',  ( -18.09353981420591140, 5.000000000000000888, -129.3374956033358387 ) ) ;
#4056 = DIRECTION ( 'NONE',  ( 0.0005249892086713290338, -0.9997374709349093891, -0.02290662775272929094 ) ) ;
#4057 = CARTESIAN_POINT ( 'NONE',  ( 1.346194077712558057, 12.56250000000000000, -6.750000000000000000 ) ) ;
#4058 = FACE_OUTER_BOUND ( 'NONE', #6748, .T. ) ;
#4059 = CARTESIAN_POINT ( 'NONE',  ( -9.756303285186646690, 6.071532165918825619E-15, -116.2179163664056176 ) ) ;
#4060 = CARTESIAN_POINT ( 'NONE',  ( 8.300023318320116417, 5.000000000000000888, -113.4762057881877553 ) ) ;
#4061 = AXIS2_PLACEMENT_3D ( 'NONE', #4545, #11564, #13748 ) ;
#4062 = CC_DESIGN_PERSON_AND_ORGANIZATION_ASSIGNMENT ( #8702, #6146, ( #12333 ) ) ;
#4063 = DIRECTION ( 'NONE',  ( 0.6182966555592911417, -2.145147447033295961E-16, 0.7859448108640934016 ) ) ;
#4064 = CIRCLE ( 'NONE', #14685, 2.500000000000002220 ) ;
#4065 = CARTESIAN_POINT ( 'NONE',  ( 4.492499072540838689, 5.000000000000000000, -2.611025101989581820 ) ) ;
#4066 = ORIENTED_EDGE ( 'NONE', *, *, #2714, .F. ) ;
#4067 = CARTESIAN_POINT ( 'NONE',  ( 8.937017960089326252, 10.66147458959636296, 2.788040780850042921 ) ) ;
#4068 = CARTESIAN_POINT ( 'NONE',  ( 14.67769753127737253, 2.331468351711927067E-16, 60.42036742134819605 ) ) ;
#4069 = CARTESIAN_POINT ( 'NONE',  ( -1.553300858899107073, 12.93750000000000178, -7.249999999999999112 ) ) ;
#4070 = CARTESIAN_POINT ( 'NONE',  ( 3.249999999999998224, 10.31250000000000000, -2.153805922287439945 ) ) ;
#4071 = CARTESIAN_POINT ( 'NONE',  ( -1.346194077712558945, 13.56250000000000000, -0.2500000000000002220 ) ) ;
#4072 = EDGE_LOOP ( 'NONE', ( #11467, #9318 ) ) ;
#4073 = CARTESIAN_POINT ( 'NONE',  ( 3.249999999999999112, 12.81250000000000000, -2.153805922287439945 ) ) ;
#4074 = AXIS2_PLACEMENT_3D ( 'NONE', #6784, #8085, #1364 ) ;
#4075 = CARTESIAN_POINT ( 'NONE',  ( -5.309262520577839872, 13.40945642053105225, -125.0911079416483176 ) ) ;
#4076 = B_SPLINE_CURVE_WITH_KNOTS ( 'NONE', 3,
 ( #3886, #7426, #14563, #13550, #2950, #12525 ),
 .UNSPECIFIED., .F., .F.,
 ( 4, 2, 4 ),
 ( 0.000000000000000000, 0.01347348681404525635, 0.02694697362809051269 ),
 .UNSPECIFIED. ) ;
#4077 = CARTESIAN_POINT ( 'NONE',  ( -5.349394595078559966, 14.88875107336558479, -103.6307550927674157 ) ) ;
#4078 = APPROVAL ( #10559, 'UNSPECIFIED' ) ;
#4079 = DIRECTION ( 'NONE',  ( 1.000000000000000000, 0.000000000000000000, 0.000000000000000000 ) ) ;
#4080 = COORDINATED_UNIVERSAL_TIME_OFFSET ( 0, 0, .AHEAD. ) ;
#4081 = ORIENTED_EDGE ( 'NONE', *, *, #9105, .F. ) ;
#4082 = CARTESIAN_POINT ( 'NONE',  ( 3.249999999999999556, 14.25000000000000178, -3.500000000000000000 ) ) ;
#4083 = VECTOR ( 'NONE', #12466, 1000.000000000000000 ) ;
#4084 = CARTESIAN_POINT ( 'NONE',  ( 1.553300858899105963, 12.56250000000000000, -7.250000000000000888 ) ) ;
#4085 = ORIENTED_EDGE ( 'NONE', *, *, #9243, .T. ) ;
#4086 = CARTESIAN_POINT ( 'NONE',  ( -10.29275726619092524, 0.000000000000000000, -34.56909192082969184 ) ) ;
#4087 = CARTESIAN_POINT ( 'NONE',  ( -1.553300858899107295, 1.437500000000000000, -7.250000000000000000 ) ) ;
#4088 = CYLINDRICAL_SURFACE ( 'NONE', #9871, 1.000000000000028644 ) ;
#4089 = CARTESIAN_POINT ( 'NONE',  ( 0.3875314106824880311, 1.514549583805837152, 4.389575455384494340 ) ) ;
#4090 =( BOUNDED_SURFACE ( )  B_SPLINE_SURFACE ( 3, 2, ( 
 ( #4258, #7570, #13618 ),
 ( #2940, #11280, #14862 ),
 ( #13761, #7726, #3157 ),
 ( #1628, #6341, #11055 ) ),
 .UNSPECIFIED., .F., .F., .F. ) 
 B_SPLINE_SURFACE_WITH_KNOTS ( ( 4, 4 ),
 ( 3, 3 ),
 ( 4.517782591535513426, 4.712388980384689674 ),
 ( 0.000000000000000000, 1.000000000000000000 ),
 .UNSPECIFIED. ) 
 GEOMETRIC_REPRESENTATION_ITEM ( )  RATIONAL_B_SPLINE_SURFACE ( (
 ( 1.000000000000000000, 0.9811261306835552531, 1.000000000000000000),
 ( 1.000000000000000000, 0.9936732040629523421, 1.000000000000000000),
 ( 1.000000000000000000, 1.000004256428960625, 1.000000000000000000),
 ( 1.000000000000000000, 1.000000000000000000, 1.000000000000000000) ) ) 
 REPRESENTATION_ITEM ( '' )  SURFACE ( )  );
#4091 = CARTESIAN_POINT ( 'NONE',  ( 2.651650429449552870, 2.625000000000000000, -6.151650429449554203 ) ) ;
#4092 = PERSON_AND_ORGANIZATION ( #3176, #3020 ) ;
#4093 = CARTESIAN_POINT ( 'NONE',  ( -67.45671875792822902, 14.09005178254165891, -198.5593552603520493 ) ) ;
#4094 = DIRECTION ( 'NONE',  ( 0.6918711009959939151, -0.000000000000000000, 0.7220210382022059781 ) ) ;
#4095 = ORIENTED_EDGE ( 'NONE', *, *, #10884, .F. ) ;
#4096 = CARTESIAN_POINT ( 'NONE',  ( -3.249999999999999556, 5.187500000000000888, -2.153805922287440833 ) ) ;
#4097 = CARTESIAN_POINT ( 'NONE',  ( -36.65864523137356201, 15.00000000000000355, -151.3474242096951343 ) ) ;
#4098 = CARTESIAN_POINT ( 'NONE',  ( 2.298097038856279362, 1.375000000000000000, -1.201902961143720860 ) ) ;
#4099 = B_SPLINE_CURVE_WITH_KNOTS ( 'NONE', 3,
 ( #7911, #14750, #13877, #2045, #6757, #11471, #3274, #4148, #13574, #12861 ),
 .UNSPECIFIED., .F., .F.,
 ( 4, 2, 2, 2, 4 ),
 ( 9.697399036122160616E-19, 0.0002702708960404782783, 0.0005405417920809555809, 0.0008108126881214329377, 0.001081083584161910078 ),
 .UNSPECIFIED. ) ;
#4100 = B_SPLINE_CURVE_WITH_KNOTS ( 'NONE', 3,
 ( #12978, #7969, #7156, #3542, #12692, #5852 ),
 .UNSPECIFIED., .F., .F.,
 ( 4, 2, 4 ),
 ( 1.301042606982605321E-18, 0.006940540637791391132, 0.01388108127558278053 ),
 .UNSPECIFIED. ) ;
#4101 = CARTESIAN_POINT ( 'NONE',  ( 0.000000000000000000, 11.50000000000000000, -0.2500000000000002220 ) ) ;
#4102 = CARTESIAN_POINT ( 'NONE',  ( 7.148068729939693000, 2.490287375297123962, -34.56909192082981974 ) ) ;
#4103 = CARTESIAN_POINT ( 'NONE',  ( -63.60348060676458459, 15.00000000000000000, -180.2685449772604045 ) ) ;
#4104 = CARTESIAN_POINT ( 'NONE',  ( -2.298097038856278473, 5.125000000000000000, -1.201902961143720416 ) ) ;
#4105 = CARTESIAN_POINT ( 'NONE',  ( -1.553300858899106629, 6.562500000000000888, 0.2499999999999998335 ) ) ;
#4106 = CARTESIAN_POINT ( 'NONE',  ( -2.651650429449553314, 9.375000000000000000, -6.151650429449552426 ) ) ;
#4107 = CARTESIAN_POINT ( 'NONE',  ( -3.573755135669773875, 2.540697700118000224, -1.000000000001791012 ) ) ;
#4108 = CARTESIAN_POINT ( 'NONE',  ( -4.492499072540820926, 5.000000000000000000, 2.611025101989610686 ) ) ;
#4109 = CARTESIAN_POINT ( 'NONE',  ( -3.750000000000000000, 8.812500000000001776, -5.053300858899105741 ) ) ;
#4110 = CARTESIAN_POINT ( 'NONE',  ( 4.856804767888951879, 14.90536770052154303, -1.840041787218201108 ) ) ;
#4111 = CARTESIAN_POINT ( 'NONE',  ( 12.51486264971105733, 2.933442265364648804, -166.3745327125327833 ) ) ;
#4112 = CARTESIAN_POINT ( 'NONE',  ( 9.173792667211671414, 1.005434785423204858, -106.2279553762535755 ) ) ;
#4113 = CARTESIAN_POINT ( 'NONE',  ( -29.53813527096436431, 1.100700607699333011E-12, -197.6188592682773333 ) ) ;
#4114 = CARTESIAN_POINT ( 'NONE',  ( 1.346194077712560944, 14.93750000000000178, -0.2500000000000010547 ) ) ;
#4115 = ADVANCED_FACE ( 'NONE', ( #13433 ), #7823, .T. ) ;
#4116 = CARTESIAN_POINT ( 'NONE',  ( -36.12930860108175324, 15.00000000000000000, -156.3173234978368953 ) ) ;
#4117 = ADVANCED_FACE ( 'NONE', ( #9225 ), #11638, .T. ) ;
#4118 = CARTESIAN_POINT ( 'NONE',  ( 3.749999999999999556, 13.25000000000000000, -3.500000000000000444 ) ) ;
#4119 = VERTEX_POINT ( 'NONE', #14974 ) ;
#4120 = FACE_OUTER_BOUND ( 'NONE', #2667, .T. ) ;
#4121 = CARTESIAN_POINT ( 'NONE',  ( 8.475206276408092876, 0.000000000000000000, -34.56909192082981974 ) ) ;
#4122 = CARTESIAN_POINT ( 'NONE',  ( -3.750000000000000000, 11.25000000000000000, -3.499999999999999112 ) ) ;
#4123 = CARTESIAN_POINT ( 'NONE',  ( -3.750000000000000000, 9.687500000000000000, -1.946699141100893149 ) ) ;
#4124 = CARTESIAN_POINT ( 'NONE',  ( -3.686330242103970978, 9.945035726838405310, -47.56170239355795104 ) ) ;
#4125 = CARTESIAN_POINT ( 'NONE',  ( -1.346194077712558945, 8.562500000000001776, -0.2500000000000002220 ) ) ;
#4126 = CARTESIAN_POINT ( 'NONE',  ( 3.749999999999999112, 12.81250000000000000, -1.946699141100892039 ) ) ;
#4127 = CARTESIAN_POINT ( 'NONE',  ( 11.00345249570077044, 12.49999999999999822, -46.06582701958618742 ) ) ;
#4128 = CC_DESIGN_PERSON_AND_ORGANIZATION_ASSIGNMENT ( #6079, #10797, ( #8443 ) ) ;
#4129 = CARTESIAN_POINT ( 'NONE',  ( -14.59253236707263213, 5.000000000000000000, -133.7561938577802891 ) ) ;
#4130 = DATE_AND_TIME ( #5127, #4259 ) ;
#4131 = CARTESIAN_POINT ( 'NONE',  ( 3.249999999999999112, 12.81250000000000000, -2.153805922287439945 ) ) ;
#4132 = CARTESIAN_POINT ( 'NONE',  ( -4.507463604512252253, 5.000000000000000000, -2.585105772303598393 ) ) ;
#4133 = DIRECTION ( 'NONE',  ( -0.000000000000000000, -1.000000000000000000, -0.000000000000000000 ) ) ;
#4134 = CARTESIAN_POINT ( 'NONE',  ( 4.532353106082944727, 1.734723475976807094E-15, -107.9759262171523204 ) ) ;
#4135 = CARTESIAN_POINT ( 'NONE',  ( 37.32986759126112730, 0.000000000000000000, 43.04214087805580391 ) ) ;
#4136 = CARTESIAN_POINT ( 'NONE',  ( 10.99551757066058322, 11.56847231179307478, -45.70224318734323532 ) ) ;
#4137 = ORIENTED_EDGE ( 'NONE', *, *, #11859, .F. ) ;
#4138 = EDGE_CURVE ( 'NONE', #4565, #9696, #4458, .T. ) ;
#4139 = CARTESIAN_POINT ( 'NONE',  ( 8.946941325060613792, 11.53387151411719103, 2.333345235934940476 ) ) ;
#4140 = DIRECTION ( 'NONE',  ( -0.000000000000000000, -1.000000000000000000, -0.000000000000000000 ) ) ;
#4141 = CARTESIAN_POINT ( 'NONE',  ( 3.749999999999999112, 12.31250000000000178, -1.946699141100893149 ) ) ;
#4142 = CARTESIAN_POINT ( 'NONE',  ( 2.298097038856279362, 10.37500000000000000, -1.201902961143720860 ) ) ;
#4143 = EDGE_CURVE ( 'NONE', #10703, #8603, #14845, .T. ) ;
#4144 = CARTESIAN_POINT ( 'NONE',  ( -3.249999999999999112, 12.81250000000000178, -4.846194077712558723 ) ) ;
#4145 = VERTEX_POINT ( 'NONE', #3351 ) ;
#4146 = AXIS2_PLACEMENT_3D ( 'NONE', #14662, #4285, #1957 ) ;
#4147 = CARTESIAN_POINT ( 'NONE',  ( 3.249999999999998668, 11.68750000000000000, -4.846194077712560500 ) ) ;
#4148 = CARTESIAN_POINT ( 'NONE',  ( -2.894564284656305553, -2.254417391461273734, -1.000000000000001110 ) ) ;
#4149 = CARTESIAN_POINT ( 'NONE',  ( -4.090890948359604984, 15.00000000000000000, -103.1929727064838147 ) ) ;
#4150 = DIRECTION ( 'NONE',  ( 0.000000000000000000, 0.000000000000000000, -1.000000000000000000 ) ) ;
#4151 = CARTESIAN_POINT ( 'NONE',  ( -7.409205697916631195, 14.09412780555631706, -116.8849570398035240 ) ) ;
#4152 = CALENDAR_DATE ( 2026, 8, 10 ) ;
#4153 = CARTESIAN_POINT ( 'NONE',  ( 8.110048856218389446, 15.00000000000000000, -122.2108563474139800 ) ) ;
#4154 = EDGE_LOOP ( 'NONE', ( #12727, #7985, #10683, #5749, #3412, #10129 ) ) ;
#4155 = CARTESIAN_POINT ( 'NONE',  ( 0.000000000000000000, 4.000000000000000000, -0.2500000000000002220 ) ) ;
#4156 = CARTESIAN_POINT ( 'NONE',  ( 0.3766621274091715987, 0.5000000000000000000, -0.1347136637304948981 ) ) ;
#4157 = CARTESIAN_POINT ( 'NONE',  ( 2.651650429449552870, 13.62500000000000000, -6.151650429449554203 ) ) ;
#4158 = EDGE_CURVE ( 'NONE', #14745, #3581, #5443, .T. ) ;
#4159 = ORIENTED_EDGE ( 'NONE', *, *, #6501, .T. ) ;
#4160 = CARTESIAN_POINT ( 'NONE',  ( -0.9087754948914270603, 2.075239479414269894, -36.05536862169275025 ) ) ;
#4161 = CARTESIAN_POINT ( 'NONE',  ( 1.553300858899108849, 2.937500000000000444, 0.2499999999999993616 ) ) ;
#4162 = CARTESIAN_POINT ( 'NONE',  ( 7.460881341449208115, 3.483300008960984240, -21.91331374262868437 ) ) ;
#4163 = CARTESIAN_POINT ( 'NONE',  ( 0.5034979235748735515, 4.307496502786065662, 5.703130291473766711 ) ) ;
#4164 = CARTESIAN_POINT ( 'NONE',  ( 3.750000000000000000, 0.7500000000000000000, -3.500000000000000444 ) ) ;
#4165 = APPLICATION_PROTOCOL_DEFINITION ( 'international standard', 'config_control_design', 1994, #15111 ) ;
#4166 = CARTESIAN_POINT ( 'NONE',  ( 26.13050938914192756, 4.000000000000000000, -138.2605953772281566 ) ) ;
#4167 = DIRECTION ( 'NONE',  ( 0.05964429961207245307, 0.000000000000000000, 0.9982196940171964572 ) ) ;
#4168 = ORIENTED_EDGE ( 'NONE', *, *, #14458, .F. ) ;
#4169 = CARTESIAN_POINT ( 'NONE',  ( -0.2513523046203912648, 0.2269315213422933297, -0.1347136637270276993 ) ) ;
#4170 = CARTESIAN_POINT ( 'NONE',  ( -2.298097038856278029, 2.625000000000000000, -1.201902961143720638 ) ) ;
#4171 = CARTESIAN_POINT ( 'NONE',  ( -3.249999999999999556, 10.75000000000000000, -3.500000000000000000 ) ) ;
#4172 = CARTESIAN_POINT ( 'NONE',  ( -0.7311112071359824327, 9.999999999999996447, -104.2753208119124366 ) ) ;
#4173 = CARTESIAN_POINT ( 'NONE',  ( -13.68460728451510455, 7.499999999999991118, -92.46488696946715891 ) ) ;
#4174 = CARTESIAN_POINT ( 'NONE',  ( 2.298097038856279362, 5.875000000000000000, -1.201902961143720860 ) ) ;
#4175 = CARTESIAN_POINT ( 'NONE',  ( -3.750000000000000000, 5.687500000000000888, -1.946699141100893149 ) ) ;
#4176 = CARTESIAN_POINT ( 'NONE',  ( 1.553300858899108849, 8.937500000000001776, 0.2499999999999993616 ) ) ;
#4177 = CARTESIAN_POINT ( 'NONE',  ( -8.648486276335429324, 2.383983337347815201, -115.6868502166757651 ) ) ;
#4178 = ORIENTED_EDGE ( 'NONE', *, *, #8436, .T. ) ;
#4179 = CARTESIAN_POINT ( 'NONE',  ( 1.243260443319662123, 4.000000000000000000, -139.4020581015306846 ) ) ;
#4180 = CARTESIAN_POINT ( 'NONE',  ( 1.553300858899109516, 8.437500000000000000, 0.2499999999999993616 ) ) ;
#4181 = DIRECTION ( 'NONE',  ( 0.000000000000000000, 1.000000000000000000, 0.000000000000000000 ) ) ;
#4182 = CARTESIAN_POINT ( 'NONE',  ( 11.29845382488883310, 0.7750707670031977692, -164.8261590475616742 ) ) ;
#4183 = CARTESIAN_POINT ( 'NONE',  ( 10.22950345979100462, 2.100000000000000089, 14.03267466424344256 ) ) ;
#4184 = CARTESIAN_POINT ( 'NONE',  ( -23.05980621591842450, 8.673617379884035472E-16, -178.1170512941666573 ) ) ;
#4185 = CARTESIAN_POINT ( 'NONE',  ( 10.12997330464346568, 0.1923925221388024520, -164.1683766026968669 ) ) ;
#4186 = DESIGN_CONTEXT ( 'detailed design', #879, 'design' ) ;
#4187 = CARTESIAN_POINT ( 'NONE',  ( -45.49174724913770262, 15.00000000000000000, -154.5113044852771793 ) ) ;
#4188 = CARTESIAN_POINT ( 'NONE',  ( -1.553300858899106629, 12.56250000000000355, 0.2500000000000002220 ) ) ;
#4189 = ORIENTED_EDGE ( 'NONE', *, *, #3758, .T. ) ;
#4190 = FACE_OUTER_BOUND ( 'NONE', #3746, .T. ) ;
#4191 = CARTESIAN_POINT ( 'NONE',  ( 7.591307135477617152, 0.1275065550641042156, -105.3485349477005570 ) ) ;
#4192 = CARTESIAN_POINT ( 'NONE',  ( 0.000000000000000000, 10.50000000000000000, 0.2499999999999998057 ) ) ;
#4193 = CARTESIAN_POINT ( 'NONE',  ( -3.330734913716225876, 10.45930188447218967, -44.51251088684002610 ) ) ;
#4194 = CARTESIAN_POINT ( 'NONE',  ( 2.298097038856279362, 9.374999999999998224, -1.201902961143720860 ) ) ;
#4195 = EDGE_CURVE ( 'NONE', #4565, #9274, #1969, .T. ) ;
#4196 = DIRECTION ( 'NONE',  ( 0.000000000000000000, 0.000000000000000000, -1.000000000000000000 ) ) ;
#4197 = CARTESIAN_POINT ( 'NONE',  ( 0.000000000000000000, 12.00000000000000000, 0.2500000000000002220 ) ) ;
#4198 = DIRECTION ( 'NONE',  ( 1.000000000000000000, 0.000000000000000000, 0.000000000000000000 ) ) ;
#4199 = CARTESIAN_POINT ( 'NONE',  ( -25.82983890416511841, 15.00000000000000000, -142.4527639562402328 ) ) ;
#4200 = ADVANCED_FACE ( 'NONE', ( #6684 ), #4702, .T. ) ;
#4201 = CARTESIAN_POINT ( 'NONE',  ( 3.249999999999999556, 12.75000000000000178, -3.500000000000000000 ) ) ;
#4202 = CARTESIAN_POINT ( 'NONE',  ( -5.619345720332211691, 10.00000000000000355, -110.1466364959252786 ) ) ;
#4203 = SECURITY_CLASSIFICATION ( '', '', #595 ) ;
#4204 = CARTESIAN_POINT ( 'NONE',  ( -0.3766621274091715987, 0.5000000000000000000, 0.1491815183709511716 ) ) ;
#4205 = CARTESIAN_POINT ( 'NONE',  ( 0.000000000000000000, 7.000000000000000000, -0.2500000000000002220 ) ) ;
#4206 = AXIS2_PLACEMENT_3D ( 'NONE', #11477, #10472, #3426 ) ;
#4207 = CARTESIAN_POINT ( 'NONE',  ( 2.930385861258905322, 0.6578274304494683422, 2.716317821862583859 ) ) ;
#4208 = CARTESIAN_POINT ( 'NONE',  ( 4.999961331844611223, 1.213798585976041210E-15, -31.08261130664305938 ) ) ;
#4209 = ORIENTED_EDGE ( 'NONE', *, *, #7305, .T. ) ;
#4210 = CARTESIAN_POINT ( 'NONE',  ( 8.957197456629506505, 11.99561947282018437, 1.863402092058872528 ) ) ;
#4211 = CARTESIAN_POINT ( 'NONE',  ( 2.860422134859788024, 14.99999999999999645, -108.4900984580837502 ) ) ;
#4212 = CARTESIAN_POINT ( 'NONE',  ( 0.000000000000000000, 3.061616997868383018E-17, 0.2500000000000002220 ) ) ;
#4213 = CARTESIAN_POINT ( 'NONE',  ( 1.346194077712561166, 11.43750000000000178, -0.2500000000000011102 ) ) ;
#4214 = CARTESIAN_POINT ( 'NONE',  ( -2.298097038856278473, 1.125000000000000222, -1.201902961143720416 ) ) ;
#4215 = ORIENTED_EDGE ( 'NONE', *, *, #4989, .T. ) ;
#4216 = CARTESIAN_POINT ( 'NONE',  ( -3.249999999999999556, 11.25000000000000000, -3.499999999999999556 ) ) ;
#4217 = APPROVAL_PERSON_ORGANIZATION ( #3277, #2152, #6762 ) ;
#4218 = CARTESIAN_POINT ( 'NONE',  ( -0.3766621274091715987, -0.1687972351630583345, 0.1491815183709511161 ) ) ;
#4219 = FACE_OUTER_BOUND ( 'NONE', #5821, .T. ) ;
#4220 = EDGE_CURVE ( 'NONE', #5312, #8297, #13602, .T. ) ;
#4221 = CARTESIAN_POINT ( 'NONE',  ( -24.61436772009224327, 4.000000000000000000, -208.9121151917288728 ) ) ;
#4222 = CARTESIAN_POINT ( 'NONE',  ( -9.486278975406271741, 11.85996688994955939, -115.8846352400755819 ) ) ;
#4223 = EDGE_CURVE ( 'NONE', #13403, #6054, #2978, .T. ) ;
#4224 = MECHANICAL_CONTEXT ( 'NONE', #12422, 'mechanical' ) ;
#4225 = CARTESIAN_POINT ( 'NONE',  ( 6.088601725813743037, 15.00000000000000000, -116.7323803970391225 ) ) ;
#4226 = CARTESIAN_POINT ( 'NONE',  ( 24.58980970989934534, 1.007048232791107889, -138.5289917632123888 ) ) ;
#4227 = ORIENTED_EDGE ( 'NONE', *, *, #14342, .T. ) ;
#4228 = CIRCLE ( 'NONE', #1243, 1.000000000000000888 ) ;
#4229 = CARTESIAN_POINT ( 'NONE',  ( -2.298097038856278473, 4.125000000000000000, -1.201902961143720416 ) ) ;
#4230 = CARTESIAN_POINT ( 'NONE',  ( -5.778809769431745735, 4.000000000000000000, -144.4900924413740313 ) ) ;
#4231 = CARTESIAN_POINT ( 'NONE',  ( 2.651650429449552870, 3.125000000000000444, -6.151650429449555091 ) ) ;
#4232 = VECTOR ( 'NONE', #544, 1000.000000000000000 ) ;
#4233 = EDGE_LOOP ( 'NONE', ( #4829, #12087, #3146, #6571, #4825, #828, #68, #2833, #2347, #3044, #1365, #8345 ) ) ;
#4234 = FACE_OUTER_BOUND ( 'NONE', #1909, .T. ) ;
#4235 = CARTESIAN_POINT ( 'NONE',  ( -3.749999999999999556, 1.312500000000000444, -5.053300858899104853 ) ) ;
#4236 = TOROIDAL_SURFACE ( 'NONE', #1017, 3.750000000000003553, 0.5000000000000000000 ) ;
#4237 = CARTESIAN_POINT ( 'NONE',  ( 7.402595682379108588, 3.357345713539126031, -22.18559871638025882 ) ) ;
#4238 = ADVANCED_FACE ( 'NONE', ( #14181 ), #13253, .T. ) ;
#4239 = CARTESIAN_POINT ( 'NONE',  ( 0.09758847591599836835, -0.03653965946317055263, 1.105386471401409443 ) ) ;
#4240 = CARTESIAN_POINT ( 'NONE',  ( -3.750000000000000000, 0.2500000000000000555, -3.499999999999999112 ) ) ;
#4241 = ADVANCED_FACE ( 'NONE', ( #4741 ), #13016, .F. ) ;
#4242 = DATE_TIME_ROLE ( 'classification_date' ) ;
#4243 = EDGE_CURVE ( 'NONE', #914, #6835, #14087, .T. ) ;
#4244 = CARTESIAN_POINT ( 'NONE',  ( 0.5944212552585367293, 6.000000000000000000, -138.5540974747773930 ) ) ;
#4245 = AXIS2_PLACEMENT_3D ( 'NONE', #3255, #6959, #9129 ) ;
#4246 = DIRECTION ( 'NONE',  ( 0.000000000000000000, -1.000000000000000000, 0.000000000000000000 ) ) ;
#4247 = ORIENTED_EDGE ( 'NONE', *, *, #4420, .T. ) ;
#4248 = DIRECTION ( 'NONE',  ( 0.000000000000000000, 1.000000000000000000, 0.000000000000000000 ) ) ;
#4249 = CARTESIAN_POINT ( 'NONE',  ( -3.249999999999999556, 1.750000000000000000, -3.500000000000000000 ) ) ;
#4250 = VECTOR ( 'NONE', #6535, 1000.000000000000227 ) ;
#4251 = CYLINDRICAL_SURFACE ( 'NONE', #11181, 3.500000000000003109 ) ;
#4252 = CARTESIAN_POINT ( 'NONE',  ( 10.98443295445820134, 13.18102764312297381, -107.0804917692757812 ) ) ;
#4253 = CARTESIAN_POINT ( 'NONE',  ( -1.553300858899107073, 6.937500000000001776, -7.249999999999999112 ) ) ;
#4254 = CARTESIAN_POINT ( 'NONE',  ( -4.592425496802573972E-16, 10.50000000000000000, -7.249999999999999112 ) ) ;
#4255 = CARTESIAN_POINT ( 'NONE',  ( -7.548446295636292547, 1.142345851352394304, -116.1647996692329343 ) ) ;
#4256 = DIRECTION ( 'NONE',  ( 0.9989498407774362043, 0.000000000000000000, 0.04581719776170026237 ) ) ;
#4257 = CARTESIAN_POINT ( 'NONE',  ( -2.651650429449552870, 8.624999999999998224, -0.8483495705504463524 ) ) ;
#4258 = CARTESIAN_POINT ( 'NONE',  ( 4.033098156699469250, 0.09438068890153242241, -1.663700395152505118 ) ) ;
#4259 = LOCAL_TIME ( 12, 28, 20.00000000000000000, #14731 ) ;
#4260 = CARTESIAN_POINT ( 'NONE',  ( 5.826207324873307059, 15.00000000000000711, -114.9748398223660075 ) ) ;
#4261 = CARTESIAN_POINT ( 'NONE',  ( 11.32016196459912649, 12.49999999999999822, -106.4092894470390291 ) ) ;
#4262 = EDGE_LOOP ( 'NONE', ( #3514, #15041, #94, #5133 ) ) ;
#4263 = CARTESIAN_POINT ( 'NONE',  ( -30.57574746150116596, 4.000000000000477840, -189.7345312606148582 ) ) ;
#4264 = CARTESIAN_POINT ( 'NONE',  ( -17.32624372123753886, 9.999999999999998224, -122.3796757791585321 ) ) ;
#4265 = CARTESIAN_POINT ( 'NONE',  ( -41.55509581774215633, 15.00000000000000000, -158.0567977604056011 ) ) ;
#4266 = CARTESIAN_POINT ( 'NONE',  ( -2.298097038856278029, 1.625000000000000000, -1.201902961143720638 ) ) ;
#4267 = ORIENTED_EDGE ( 'NONE', *, *, #9690, .T. ) ;
#4268 = CYLINDRICAL_SURFACE ( 'NONE', #1091, 1.000000000000042633 ) ;
#4269 = CARTESIAN_POINT ( 'NONE',  ( 10.04877821836624996, 1.662336431860132357, -106.0315262505607450 ) ) ;
#4270 = DIRECTION ( 'NONE',  ( -0.000000000000000000, -1.000000000000000000, -0.000000000000000000 ) ) ;
#4271 = CARTESIAN_POINT ( 'NONE',  ( -15.55390927925940758, 8.673617379884033500E-16, -185.3651796119466439 ) ) ;
#4272 = CARTESIAN_POINT ( 'NONE',  ( -3.294555838739222420, 5.000000000000000888, -108.9576586820894732 ) ) ;
#4273 = CARTESIAN_POINT ( 'NONE',  ( 3.249999999999998224, 9.312500000000001776, -2.153805922287439945 ) ) ;
#4274 = CARTESIAN_POINT ( 'NONE',  ( 0.2499999999999999445, 4.500000000000000888, 1.500000000000000222 ) ) ;
#4275 = CARTESIAN_POINT ( 'NONE',  ( 3.750000000000000000, 14.75000000000000178, -3.500000000000000444 ) ) ;
#4276 = AXIS2_PLACEMENT_3D ( 'NONE', #10281, #15246, #1006 ) ;
#4277 = CARTESIAN_POINT ( 'NONE',  ( -7.229287782379126170, 13.81375925440817731, -104.6456827072011038 ) ) ;
#4278 = CARTESIAN_POINT ( 'NONE',  ( 1.346194077712560944, 11.93750000000000000, -0.2500000000000010547 ) ) ;
#4279 = CARTESIAN_POINT ( 'NONE',  ( -5.488578029460351004, 2.529993217055222399, -43.69424231201528386 ) ) ;
#4280 = DIRECTION ( 'NONE',  ( 0.000000000000000000, 0.000000000000000000, 1.000000000000000000 ) ) ;
#4281 = CARTESIAN_POINT ( 'NONE',  ( -2.298097038856278918, 9.375000000000000000, -5.798097038856277585 ) ) ;
#4282 = FACE_OUTER_BOUND ( 'NONE', #13981, .T. ) ;
#4283 = CARTESIAN_POINT ( 'NONE',  ( -7.751437813422534795, 5.000000000000000000, -124.5369783794910319 ) ) ;
#4284 = ORIENTED_EDGE ( 'NONE', *, *, #13361, .F. ) ;
#4285 = DIRECTION ( 'NONE',  ( 0.000000000000000000, 1.000000000000000000, 0.000000000000000000 ) ) ;
#4286 = PERSON ( 'NAUO-PER4', 'UNSPECIFIED', 'UNSPECIFIED', ('UNSPECIFIED'), ('UNSPECIFIED'), ('UNSPECIFIED') ) ;
#4287 = CARTESIAN_POINT ( 'NONE',  ( 13.63124210137304537, 12.50000000000000000, -125.8318412418369121 ) ) ;
#4288 = CARTESIAN_POINT ( 'NONE',  ( -3.749999999999999556, 1.187500000000000444, -1.946699141100892927 ) ) ;
#4289 = AXIS2_PLACEMENT_3D ( 'NONE', #4021, #10971, #9811 ) ;
#4290 = CARTESIAN_POINT ( 'NONE',  ( 1.346194077712561166, 14.43750000000000178, -0.2500000000000011102 ) ) ;
#4291 = CARTESIAN_POINT ( 'NONE',  ( -3.249999999999999556, 0.3125000000000000555, -4.846194077712557835 ) ) ;
#4292 = EDGE_LOOP ( 'NONE', ( #12251, #1707, #5675, #102 ) ) ;
#4293 = CARTESIAN_POINT ( 'NONE',  ( 2.298097038856278473, 10.62500000000000000, -5.798097038856279362 ) ) ;
#4294 = CARTESIAN_POINT ( 'NONE',  ( 9.940211158120410673, 12.49999999999999645, -43.17897536272746351 ) ) ;
#4295 = DIRECTION ( 'NONE',  ( 0.000000000000000000, -1.000000000000000000, -0.000000000000000000 ) ) ;
#4296 = DIRECTION ( 'NONE',  ( 1.000000000000000000, 0.000000000000000000, -0.000000000000000000 ) ) ;
#4297 = CARTESIAN_POINT ( 'NONE',  ( -9.385448347264278013, 10.00000000000000000, -115.3551636530117293 ) ) ;
#4298 = VECTOR ( 'NONE', #11292, 1000.000000000000000 ) ;
#4299 = DATE_AND_TIME ( #4152, #14590 ) ;
#4300 = AXIS2_PLACEMENT_3D ( 'NONE', #9011, #3289, #13584 ) ;
#4301 = CARTESIAN_POINT ( 'NONE',  ( 9.815018941082433557, 15.00000000000000000, -124.9446060552849218 ) ) ;
#4302 = DIRECTION ( 'NONE',  ( 0.000000000000000000, 0.000000000000000000, 1.000000000000000000 ) ) ;
#4303 = CARTESIAN_POINT ( 'NONE',  ( 26.71007981443008816, 5.000000000000001776, -136.8791680534697832 ) ) ;
#4304 = ORIENTED_EDGE ( 'NONE', *, *, #10792, .T. ) ;
#4305 = CARTESIAN_POINT ( 'NONE',  ( -2.298097038856278473, 6.125000000000000000, -1.201902961143720416 ) ) ;
#4306 = LINE ( 'NONE', #4156, #13679 ) ;
#4307 = CARTESIAN_POINT ( 'NONE',  ( 1.553300858899109516, 3.437500000000000444, 0.2499999999999993616 ) ) ;
#4308 = EDGE_LOOP ( 'NONE', ( #2280, #4637, #4365, #2926, #12759, #7898, #4449 ) ) ;
#4309 = EDGE_CURVE ( 'NONE', #8407, #10451, #14251, .T. ) ;
#4310 = CARTESIAN_POINT ( 'NONE',  ( 13.77177382422822838, 1.749999999999351186, 61.31538778292295433 ) ) ;
#4311 = AXIS2_PLACEMENT_3D ( 'NONE', #8331, #6680, #14385 ) ;
#4312 = CARTESIAN_POINT ( 'NONE',  ( -1.726026643059569432, 7.379999999999995453, -47.97842334616509419 ) ) ;
#4313 = CARTESIAN_POINT ( 'NONE',  ( 0.000000000000000000, 7.000000000000000000, 0.2500000000000002220 ) ) ;
#4314 = CARTESIAN_POINT ( 'NONE',  ( -63.84839510230030868, 9.999999999999998224, -211.4757795387517945 ) ) ;
#4315 = LINE ( 'NONE', #9019, #10169 ) ;
#4316 = CARTESIAN_POINT ( 'NONE',  ( 2.651650429449553759, 2.875000000000000000, -0.8483495705504471296 ) ) ;
#4317 = DATE_AND_TIME ( #11496, #11168 ) ;
#4318 = CARTESIAN_POINT ( 'NONE',  ( 22.16272538625586108, 5.000000000000000888, -133.7353905083487575 ) ) ;
#4319 = AXIS2_PLACEMENT_3D ( 'NONE', #8834, #12308, #653 ) ;
#4320 = FACE_OUTER_BOUND ( 'NONE', #115, .T. ) ;
#4321 = ORIENTED_EDGE ( 'NONE', *, *, #6013, .F. ) ;
#4322 = DIRECTION ( 'NONE',  ( 0.000000000000000000, 0.000000000000000000, -1.000000000000000000 ) ) ;
#4323 = CARTESIAN_POINT ( 'NONE',  ( 2.298097038856279362, 3.375000000000000444, -1.201902961143720860 ) ) ;
#4324 = CARTESIAN_POINT ( 'NONE',  ( 10.74700110368927675, 13.76866009450032458, -106.9415428707061295 ) ) ;
#4325 = ADVANCED_FACE ( 'NONE', ( #1183 ), #5885, .F. ) ;
#4326 = CARTESIAN_POINT ( 'NONE',  ( -5.307246684019970573, 4.336808689942017736E-16, -122.2414390436973122 ) ) ;
#4327 = CARTESIAN_POINT ( 'NONE',  ( -3.750000000000000000, 7.687500000000000000, -1.946699141100893149 ) ) ;
#4328 = CARTESIAN_POINT ( 'NONE',  ( -3.750000000000000000, 12.25000000000000000, -3.499999999999999112 ) ) ;
#4329 = CARTESIAN_POINT ( 'NONE',  ( -6.442579204135247650, 0.4622145201094847722, -116.6257450304696874 ) ) ;
#4330 = VERTEX_POINT ( 'NONE', #2658 ) ;
#4331 = CARTESIAN_POINT ( 'NONE',  ( -4.580007248825209487, 7.420008617947661109E-16, -117.4298695725520929 ) ) ;
#4332 = CARTESIAN_POINT ( 'NONE',  ( -3.749999999999999556, 8.750000000000000000, -3.499999999999999112 ) ) ;
#4333 = CARTESIAN_POINT ( 'NONE',  ( -5.813238319161563972, 2.708338984294549324E-32, -104.9413748694892661 ) ) ;
#4334 = CARTESIAN_POINT ( 'NONE',  ( 6.147223190827659778, 15.00000000000000000, -110.9794920126036004 ) ) ;
#4335 = DIRECTION ( 'NONE',  ( -0.02181900108494679719, 0.000000000000000000, 0.9997619372588931741 ) ) ;
#4336 = ORIENTED_EDGE ( 'NONE', *, *, #14445, .F. ) ;
#4337 = CARTESIAN_POINT ( 'NONE',  ( -29.65136226273812170, 8.190558003531155927E-13, -196.7288660786858827 ) ) ;
#4338 = DIRECTION ( 'NONE',  ( 0.08794243244723007336, 0.000000000000000000, 0.9961255586397049777 ) ) ;
#4339 = CARTESIAN_POINT ( 'NONE',  ( -42.37771161474321957, 9.999999999999998224, -158.4861704487694567 ) ) ;
#4340 = CARTESIAN_POINT ( 'NONE',  ( 0.000000000000000000, 1.500000000000000222, -0.2500000000000002220 ) ) ;
#4341 = VERTEX_POINT ( 'NONE', #2418 ) ;
#4342 = CARTESIAN_POINT ( 'NONE',  ( 7.220173501946012706, 4.999999999999999112, -111.8642345870615458 ) ) ;
#4343 = CARTESIAN_POINT ( 'NONE',  ( 6.288457687488933523, 0.000000000000000000, -105.0111312234435985 ) ) ;
#4344 = EDGE_CURVE ( 'NONE', #11904, #5461, #11837, .T. ) ;
#4345 = CARTESIAN_POINT ( 'NONE',  ( 2.222606327602053788, 15.00000000000000178, -129.3650357598043001 ) ) ;
#4346 = CARTESIAN_POINT ( 'NONE',  ( 8.942877807459197470, 11.25919951447419010, 2.519538463272103179 ) ) ;
#4347 = CARTESIAN_POINT ( 'NONE',  ( -4.869293993580057212, 1.734723475976807094E-15, -118.1204535358569530 ) ) ;
#4348 = CARTESIAN_POINT ( 'NONE',  ( -2.298097038856279362, 7.874999999999999112, -5.798097038856278473 ) ) ;
#4349 = CARTESIAN_POINT ( 'NONE',  ( -3.749999999999999556, -0.2499999999999998890, -3.499999999999999112 ) ) ;
#4350 = CARTESIAN_POINT ( 'NONE',  ( 10.95001698349728336, 5.943472311793079221, -43.61737436169475046 ) ) ;
#4351 = CYLINDRICAL_SURFACE ( 'NONE', #509, 3.000000000000011990 ) ;
#4352 = CARTESIAN_POINT ( 'NONE',  ( -1.346194077712559389, 11.43750000000000000, -6.749999999999999112 ) ) ;
#4353 = CARTESIAN_POINT ( 'NONE',  ( -8.886921396801742645, 9.999999999999998224, -105.5168766094550676 ) ) ;
#4354 = DIRECTION ( 'NONE',  ( -0.000000000000000000, -1.000000000000000000, -0.000000000000000000 ) ) ;
#4355 = CARTESIAN_POINT ( 'NONE',  ( 1.346194077712558057, 8.562500000000001776, -6.750000000000000000 ) ) ;
#4356 = CARTESIAN_POINT ( 'NONE',  ( 0.5805642473066149334, -4.817921077453451975E-12, -138.6354391049652293 ) ) ;
#4357 = LINE ( 'NONE', #10231, #11830 ) ;
#4358 = VERTEX_POINT ( 'NONE', #5966 ) ;
#4359 = CARTESIAN_POINT ( 'NONE',  ( 10.95001698349729047, 5.943472311793079221, -43.61737436169475046 ) ) ;
#4360 = CARTESIAN_POINT ( 'NONE',  ( 8.672589136283018973, 12.50000000000000000, -116.8319891675733828 ) ) ;
#4361 = CARTESIAN_POINT ( 'NONE',  ( 1.553300858899109071, 15.43750000000000178, 0.2499999999999989175 ) ) ;
#4362 = CARTESIAN_POINT ( 'NONE',  ( 3.749999999999999556, 1.249999999999999778, -3.500000000000000444 ) ) ;
#4363 = EDGE_CURVE ( 'NONE', #11204, #14187, #5684, .T. ) ;
#4364 = CARTESIAN_POINT ( 'NONE',  ( -3.249999999999999556, 1.312500000000000444, -4.846194077712557835 ) ) ;
#4365 = ORIENTED_EDGE ( 'NONE', *, *, #8374, .F. ) ;
#4366 = CARTESIAN_POINT ( 'NONE',  ( 0.000000000000000000, 10.00000000000000000, -0.2500000000000002220 ) ) ;
#4367 = CARTESIAN_POINT ( 'NONE',  ( 0.000000000000000000, 1.000000000000000000, 0.000000000000000000 ) ) ;
#4368 = CARTESIAN_POINT ( 'NONE',  ( -8.651269111992894167, 12.39895203580364047, -104.9132380198166885 ) ) ;
#4369 =( NAMED_UNIT ( * ) PLANE_ANGLE_UNIT ( ) SI_UNIT ( $, .RADIAN. ) );
#4370 = CARTESIAN_POINT ( 'NONE',  ( 0.000000000000000000, 15.00000000000000000, -0.2500000000000002220 ) ) ;
#4371 = APPROVAL_ROLE ( '' ) ;
#4372 = CARTESIAN_POINT ( 'NONE',  ( 11.32055997317818985, 15.00000000000186517, -122.6997364776348576 ) ) ;
#4373 = CARTESIAN_POINT ( 'NONE',  ( -5.599106598293994708, 14.85395790697270257, -117.2453520682029904 ) ) ;
#4374 = CARTESIAN_POINT ( 'NONE',  ( 0.2625675448779695720, 5.000000000000000888, 2.974107436473219401 ) ) ;
#4375 = CARTESIAN_POINT ( 'NONE',  ( -3.249999999999999556, 11.18750000000000000, -2.153805922287440833 ) ) ;
#4376 = ORIENTED_EDGE ( 'NONE', *, *, #14699, .F. ) ;
#4377 = CARTESIAN_POINT ( 'NONE',  ( -1.346194077712559389, 5.437500000000002665, -6.749999999999999112 ) ) ;
#4378 = CARTESIAN_POINT ( 'NONE',  ( -1.713579061006052839, 4.000000000000000000, -141.3534686916246983 ) ) ;
#4379 = CARTESIAN_POINT ( 'NONE',  ( 1.553300858899105963, 0.06250000000000016653, -7.250000000000000888 ) ) ;
#4380 = VECTOR ( 'NONE', #10226, 1000.000000000000000 ) ;
#4381 = ORIENTED_EDGE ( 'NONE', *, *, #11293, .F. ) ;
#4382 = CARTESIAN_POINT ( 'NONE',  ( -9.385448347264265578, 10.35017622395433357, -115.3551636530117719 ) ) ;
#4383 = CARTESIAN_POINT ( 'NONE',  ( -3.249999999999999556, 0.3125000000000000555, -4.846194077712557835 ) ) ;
#4384 = CARTESIAN_POINT ( 'NONE',  ( 3.750000000000000000, 5.750000000000000000, -3.500000000000000444 ) ) ;
#4385 = EDGE_CURVE ( 'NONE', #13160, #7071, #4942, .T. ) ;
#4386 = CARTESIAN_POINT ( 'NONE',  ( -25.63704293604745743, 1.707693810710474880, -207.0033111944292727 ) ) ;
#4387 = CARTESIAN_POINT ( 'NONE',  ( 3.226532413654821685, 4.345304807832050642, 5.176332484491082297 ) ) ;
#4388 = COORDINATED_UNIVERSAL_TIME_OFFSET ( 0, 0, .AHEAD. ) ;
#4389 = EDGE_CURVE ( 'NONE', #5529, #6819, #10372, .T. ) ;
#4390 = DIRECTION ( 'NONE',  ( -0.02181900108494696719, 0.000000000000000000, 0.9997619372588931741 ) ) ;
#4391 = VERTEX_POINT ( 'NONE', #7439 ) ;
#4392 = CARTESIAN_POINT ( 'NONE',  ( 3.249999999999999556, 3.250000000000000000, -3.500000000000000000 ) ) ;
#4393 = CARTESIAN_POINT ( 'NONE',  ( 11.04730217088350663, 12.49999999999999822, -107.1178495010082941 ) ) ;
#4394 = SHAPE_REPRESENTATION ( 'ShearsLockingLatch_Predeterminado', ( #9419 ), #14368 ) ;
#4395 = CARTESIAN_POINT ( 'NONE',  ( 2.651650429449553314, 9.374999999999998224, -0.8483495705504476847 ) ) ;
#4396 = CARTESIAN_POINT ( 'NONE',  ( -1.553300858899107073, 12.43750000000000000, -7.250000000000000000 ) ) ;
#4397 = CARTESIAN_POINT ( 'NONE',  ( 1.052436484934207606, 2.529993217055222843, -1.000000000000029088 ) ) ;
#4398 = CARTESIAN_POINT ( 'NONE',  ( -9.721966606378854792, 4.649066463566643215, -116.3614657639810019 ) ) ;
#4399 = CARTESIAN_POINT ( 'NONE',  ( -1.346194077712559167, 0.9375000000000002220, -6.749999999999999112 ) ) ;
#4400 = CARTESIAN_POINT ( 'NONE',  ( -24.61436772009224327, 4.000000000000000000, -208.9121151917288728 ) ) ;
#4401 = LINE ( 'NONE', #2086, #8382 ) ;
#4402 = EDGE_LOOP ( 'NONE', ( #11243, #9388, #7105, #8368, #3357, #5785 ) ) ;
#4403 = CARTESIAN_POINT ( 'NONE',  ( 5.907106717946758678, 3.280814621631571004, 4.948311739797290443 ) ) ;
#4404 = CARTESIAN_POINT ( 'NONE',  ( 1.453757729950655886, -2.743867526398025447, -1.000000000000021760 ) ) ;
#4405 = CARTESIAN_POINT ( 'NONE',  ( -37.87309319203819769, 9.999999999999998224, -156.6288150092206024 ) ) ;
#4406 = CARTESIAN_POINT ( 'NONE',  ( -3.249999999999999112, 4.687500000000000888, -2.153805922287440833 ) ) ;
#4407 = EDGE_LOOP ( 'NONE', ( #2425, #6421, #8484, #10315 ) ) ;
#4408 = CARTESIAN_POINT ( 'NONE',  ( -0.3766621274091715987, 0.5000000000000000000, -0.1347136637304948981 ) ) ;
#4409 = CARTESIAN_POINT ( 'NONE',  ( 3.717577911061880958, 0.000000000000000000, -143.6771719914432879 ) ) ;
#4410 = CARTESIAN_POINT ( 'NONE',  ( 3.249999999999998668, 10.68750000000000000, -4.846194077712560500 ) ) ;
#4411 = B_SPLINE_CURVE_WITH_KNOTS ( 'NONE', 3,
 ( #1145, #9486, #15234, #11796, #923, #2228, #8170, #2160 ),
 .UNSPECIFIED., .F., .F.,
 ( 4, 2, 2, 4 ),
 ( 0.002924603232979225333, 0.004377839289350649032, 0.005104457317536361532, 0.005831075345722074033 ),
 .UNSPECIFIED. ) ;
#4412 = CARTESIAN_POINT ( 'NONE',  ( 6.223671794703586890, 13.99084746319145722, 3.305819595603176175 ) ) ;
#4413 = FACE_OUTER_BOUND ( 'NONE', #11190, .T. ) ;
#4414 = CARTESIAN_POINT ( 'NONE',  ( 3.249999999999998224, 14.31250000000000355, -2.153805922287439945 ) ) ;
#4415 = CARTESIAN_POINT ( 'NONE',  ( 16.38488885224993652, 8.673617379884035472E-16, -147.4012479123365154 ) ) ;
#4416 = CARTESIAN_POINT ( 'NONE',  ( -2.651650429449553314, -0.1249999999999999029, -6.151650429449552426 ) ) ;
#4417 = LINE ( 'NONE', #3334, #9721 ) ;
#4418 = AXIS2_PLACEMENT_3D ( 'NONE', #14864, #7729, #631 ) ;
#4419 = DIRECTION ( 'NONE',  ( 0.000000000000000000, 0.000000000000000000, 1.000000000000000000 ) ) ;
#4420 = EDGE_CURVE ( 'NONE', #13029, #13794, #13087, .T. ) ;
#4421 = CARTESIAN_POINT ( 'NONE',  ( -8.243994158936986949, 2.500000000000000444, -104.7509493499769917 ) ) ;
#4422 = ADVANCED_FACE ( 'NONE', ( #13635 ), #13155, .T. ) ;
#4423 = CARTESIAN_POINT ( 'NONE',  ( -5.255910738709840935, 10.00000000000000178, -115.0300074718742991 ) ) ;
#4424 = EDGE_CURVE ( 'NONE', #12117, #9630, #9767, .T. ) ;
#4425 = CARTESIAN_POINT ( 'NONE',  ( -1.500000000000000000, 5.000000000000000000, 0.2500000000000002220 ) ) ;
#4426 = CARTESIAN_POINT ( 'NONE',  ( 0.000000000000000000, 8.000000000000000000, -0.2500000000000002220 ) ) ;
#4427 = CARTESIAN_POINT ( 'NONE',  ( 26.58801926426209405, 5.000000000000000888, -139.0072983920785532 ) ) ;
#4428 = DIRECTION ( 'NONE',  ( 0.000000000000000000, 1.000000000000000000, 0.000000000000000000 ) ) ;
#4429 = ORIENTED_EDGE ( 'NONE', *, *, #14828, .F. ) ;
#4430 = ORIENTED_EDGE ( 'NONE', *, *, #10144, .T. ) ;
#4431 = CARTESIAN_POINT ( 'NONE',  ( 5.000000000000000888, 15.00000000000000000, -100.6237003951525679 ) ) ;
#4432 = CARTESIAN_POINT ( 'NONE',  ( -4.592425496802573972E-16, 1.500000000000000000, -7.249999999999999112 ) ) ;
#4433 = CARTESIAN_POINT ( 'NONE',  ( 3.249999999999998224, 14.18750000000000178, -4.846194077712561388 ) ) ;
#4434 = CARTESIAN_POINT ( 'NONE',  ( -25.82983890416511841, 9.999999999999998224, -142.4527639562402328 ) ) ;
#4435 = ORIENTED_EDGE ( 'NONE', *, *, #11584, .T. ) ;
#4436 = CARTESIAN_POINT ( 'NONE',  ( 3.249999999999998668, 13.68750000000000000, -4.846194077712560500 ) ) ;
#4437 = DIRECTION ( 'NONE',  ( 1.000000000000000000, 0.000000000000000000, 0.000000000000000000 ) ) ;
#4438 = APPROVAL_PERSON_ORGANIZATION ( #12419, #2928, #685 ) ;
#4439 = CARTESIAN_POINT ( 'NONE',  ( 52.95141737058320075, 2.100000000000000089, 69.12768672987860441 ) ) ;
#4440 = CARTESIAN_POINT ( 'NONE',  ( -7.978007822725404097, 13.46737988729077706, -115.9805901612444927 ) ) ;
#4441 = VECTOR ( 'NONE', #49, 1000.000000000000227 ) ;
#4442 = APPROVAL_DATE_TIME ( #9458, #3558 ) ;
#4443 = CARTESIAN_POINT ( 'NONE',  ( 10.31224696304875010, 12.49999999999999822, -121.0233796644210429 ) ) ;
#4444 = CARTESIAN_POINT ( 'NONE',  ( -9.721966606378853015, 10.35093353643332570, -116.3614657639809309 ) ) ;
#4445 = ORIENTED_EDGE ( 'NONE', *, *, #14746, .F. ) ;
#4446 = CARTESIAN_POINT ( 'NONE',  ( 20.87131526946576443, 1.301042606982605321E-15, -138.9752963459259547 ) ) ;
#4447 = CARTESIAN_POINT ( 'NONE',  ( -3.249999999999999556, 12.25000000000000000, -3.499999999999999556 ) ) ;
#4448 = ORIENTED_EDGE ( 'NONE', *, *, #6781, .F. ) ;
#4449 = ORIENTED_EDGE ( 'NONE', *, *, #7718, .T. ) ;
#4450 = CARTESIAN_POINT ( 'NONE',  ( -1.346194077712559389, 5.062500000000001776, -0.2500000000000002220 ) ) ;
#4451 = CARTESIAN_POINT ( 'NONE',  ( 16.43549277046052026, 8.749999999999998224, -88.72346770343305877 ) ) ;
#4452 = CARTESIAN_POINT ( 'NONE',  ( 0.000000000000000000, 2.500000000000000000, 0.2500000000000002220 ) ) ;
#4453 = CARTESIAN_POINT ( 'NONE',  ( 2.298097038856278029, 6.125000000000000000, -5.798097038856279362 ) ) ;
#4454 = VERTEX_POINT ( 'NONE', #5125 ) ;
#4455 = APPROVAL_PERSON_ORGANIZATION ( #9534, #13108, #3820 ) ;
#4456 = CARTESIAN_POINT ( 'NONE',  ( -8.256868333794654902, 13.15908446542855970, -115.8592241392984477 ) ) ;
#4457 = CARTESIAN_POINT ( 'NONE',  ( 0.000000000000000000, 0.000000000000000000, 0.000000000000000000 ) ) ;
#4458 = CIRCLE ( 'NONE', #7896, 2.326940983401415419 ) ;
#4459 = CARTESIAN_POINT ( 'NONE',  ( 3.750000000000000000, 6.750000000000000000, -3.500000000000000444 ) ) ;
#4460 = CARTESIAN_POINT ( 'NONE',  ( -25.11906781955737600, 1.301042606982605321E-15, -198.9681998140721078 ) ) ;
#4461 = CARTESIAN_POINT ( 'NONE',  ( 1.050483441592383604, -6.071532165918824042E-15, -129.2792135173282873 ) ) ;
#4462 = COORDINATED_UNIVERSAL_TIME_OFFSET ( 0, 0, .AHEAD. ) ;
#4463 = AXIS2_PLACEMENT_3D ( 'NONE', #7711, #12427, #689 ) ;
#4464 = CARTESIAN_POINT ( 'NONE',  ( 9.195819311509541905, 5.000000000000000888, -109.7388120284761897 ) ) ;
#4465 = AXIS2_PLACEMENT_3D ( 'NONE', #508, #8697, #14208 ) ;
#4466 = AXIS2_PLACEMENT_3D ( 'NONE', #8947, #7629, #3075 ) ;
#4467 = ORIENTED_EDGE ( 'NONE', *, *, #2625, .F. ) ;
#4468 = CARTESIAN_POINT ( 'NONE',  ( 0.000000000000000000, 7.499999999999999112, -0.2500000000000002220 ) ) ;
#4469 = DIRECTION ( 'NONE',  ( 0.01091012466144563632, -0.002150395083030232687, -0.9999381705789908148 ) ) ;
#4470 = AXIS2_PLACEMENT_3D ( 'NONE', #644, #3253, #12378 ) ;
#4471 = CARTESIAN_POINT ( 'NONE',  ( -3.750000000000000000, 10.81250000000000000, -5.053300858899105741 ) ) ;
#4472 = CARTESIAN_POINT ( 'NONE',  ( -2.651650429449552870, 12.12500000000000000, -0.8483495705504462414 ) ) ;
#4473 = CARTESIAN_POINT ( 'NONE',  ( 6.369258321017759350, 2.529993217055222843, -34.56909192082981974 ) ) ;
#4474 = CARTESIAN_POINT ( 'NONE',  ( -0.1182668585043939180, 2.358359890833529260, -138.2405088131075956 ) ) ;
#4475 = CARTESIAN_POINT ( 'NONE',  ( 1.553300858899109516, 13.43750000000000178, 0.2499999999999993616 ) ) ;
#4476 = CARTESIAN_POINT ( 'NONE',  ( -2.638275913571042519, 4.336808689942017243E-16, -112.4126634647521570 ) ) ;
#4477 = DIRECTION ( 'NONE',  ( -0.001336022302423332114, -0.9997192698606586214, -0.02365579239170265829 ) ) ;
#4478 = PRODUCT_DEFINITION_SHAPE ( 'NONE', 'NONE',  #2439 ) ;
#4479 = CARTESIAN_POINT ( 'NONE',  ( 10.00087860767147063, 5.000000000000000888, -45.95880046359209103 ) ) ;
#4480 = CIRCLE ( 'NONE', #795, 6.999999999999950262 ) ;
#4481 = VERTEX_POINT ( 'NONE', #2815 ) ;
#4482 = FACE_OUTER_BOUND ( 'NONE', #3091, .T. ) ;
#4483 = CARTESIAN_POINT ( 'NONE',  ( -1.346194077712558945, 0.06250000000000000000, -0.2500000000000002220 ) ) ;
#4484 =( BOUNDED_SURFACE ( )  B_SPLINE_SURFACE ( 3, 2, ( 
 ( #8967, #2016, #13625 ),
 ( #6574, #9977, #15013 ),
 ( #12450, #14944, #3025 ),
 ( #10278, #6726, #5491 ),
 ( #13697, #6500, #5339 ),
 ( #14717, #1937, #1787 ),
 ( #7732, #4116, #11439 ),
 ( #4405, #861, #635 ),
 ( #556, #10210, #12675 ),
 ( #6649, #8819, #7809 ),
 ( #14869, #6418, #9114 ),
 ( #5563, #14792, #11215 ),
 ( #13840, #4265, #3242 ),
 ( #4339, #7955, #13546 ),
 ( #10055, #12521, #4187 ),
 ( #5412, #2946, #11138 ),
 ( #5268, #8892, #1869 ),
 ( #7653, #11358, #786 ),
 ( #9046, #11286, #707 ),
 ( #13768, #12597, #3163 ),
 ( #7875, #10657, #2321 ),
 ( #4635, #15089, #1002 ),
 ( #4485, #14068, #5712 ),
 ( #2168, #3470, #3322 ),
 ( #8032, #2388, #12757 ),
 ( #12829, #15169, #6800 ),
 ( #9194, #4563, #11664 ),
 ( #13924, #14149, #72 ),
 ( #2090, #8256, #10349 ),
 ( #7084, #5857, #1222 ),
 ( #6870, #11585, #11806 ),
 ( #4784, #5932, #9272 ),
 ( #9498, #10432, #8182 ),
 ( #13996, #1082, #3395 ),
 ( #12907, #14222, #8104 ),
 ( #3623, #5634, #10509 ),
 ( #2240, #11733, #6947 ),
 ( #4710, #5788, #15243 ) ),
 .UNSPECIFIED., .F., .F., .T. ) 
 B_SPLINE_SURFACE_WITH_KNOTS ( ( 4, 2, 2, 2, 2, 2, 2, 2, 2, 2, 2, 2, 2, 2, 2, 2, 2, 2, 4 ),
 ( 3, 3 ),
 ( 0.000000000000000000, 0.004617214637118580677, 0.006925821955677870581, 0.009234429274237161353, 0.01385164391135574116, 0.01500594757063538655, 0.01616025122991503193, 0.01846885854847432271, 0.02308607318559290078, 0.02770328782271148232, 0.03232050245983006387, 0.03462910977838935811, 0.03693771709694864541, 0.04617214637118580156, 0.05540657564542296465, 0.05771518296398225889, 0.06002379028254154619, 0.06464100491966012774, 0.07387543419389729082 ),
 ( 0.000000000000000000, 1.000000000000000000 ),
 .UNSPECIFIED. ) 
 GEOMETRIC_REPRESENTATION_ITEM ( )  RATIONAL_B_SPLINE_SURFACE ( (
 ( 1.000000000000000000, 0.7071067811865475727, 1.000000000000000000),
 ( 1.000000000000000000, 0.7071067811865475727, 1.000000000000000000),
 ( 1.000000000000000000, 0.7071067811865475727, 1.000000000000000000),
 ( 1.000000000000000000, 0.7071067811865475727, 1.000000000000000000),
 ( 1.000000000000000000, 0.7071067811865475727, 1.000000000000000000),
 ( 1.000000000000000000, 0.7071067811865475727, 1.000000000000000000),
 ( 1.000000000000000000, 0.7071067811865475727, 1.000000000000000000),
 ( 1.000000000000000000, 0.7071067811865475727, 1.000000000000000000),
 ( 1.000000000000000000, 0.7071067811865475727, 1.000000000000000000),
 ( 1.000000000000000000, 0.7071067811865475727, 1.000000000000000000),
 ( 1.000000000000000000, 0.7071067811865475727, 1.000000000000000000),
 ( 1.000000000000000000, 0.7071067811865475727, 1.000000000000000000),
 ( 1.000000000000000000, 0.7071067811865475727, 1.000000000000000000),
 ( 1.000000000000000000, 0.7071067811865475727, 1.000000000000000000),
 ( 1.000000000000000000, 0.7071067811865475727, 1.000000000000000000),
 ( 1.000000000000000000, 0.7071067811865475727, 1.000000000000000000),
 ( 1.000000000000000000, 0.7071067811865475727, 1.000000000000000000),
 ( 1.000000000000000000, 0.7071067811865475727, 1.000000000000000000),
 ( 1.000000000000000000, 0.7071067811865477948, 1.000000000000000000),
 ( 1.000000000000000000, 0.7071067811865477948, 1.000000000000000000),
 ( 1.000000000000000000, 0.7071067811865475727, 1.000000000000000000),
 ( 1.000000000000000000, 0.7071067811865475727, 1.000000000000000000),
 ( 1.000000000000000000, 0.7071067811865475727, 1.000000000000000000),
 ( 1.000000000000000000, 0.7071067811865475727, 1.000000000000000000),
 ( 1.000000000000000000, 0.7071067811865475727, 1.000000000000000000),
 ( 1.000000000000000000, 0.7071067811865475727, 1.000000000000000000),
 ( 1.000000000000000000, 0.7071067811865480168, 1.000000000000000000),
 ( 1.000000000000000000, 0.7071067811865480168, 1.000000000000000000),
 ( 1.000000000000000000, 0.7071067811865475727, 1.000000000000000000),
 ( 1.000000000000000000, 0.7071067811865475727, 1.000000000000000000),
 ( 1.000000000000000000, 0.7071067811865475727, 1.000000000000000000),
 ( 1.000000000000000000, 0.7071067811865475727, 1.000000000000000000),
 ( 1.000000000000000000, 0.7071067811865475727, 1.000000000000000000),
 ( 1.000000000000000000, 0.7071067811865475727, 1.000000000000000000),
 ( 1.000000000000000000, 0.7071067811865475727, 1.000000000000000000),
 ( 1.000000000000000000, 0.7071067811865475727, 1.000000000000000000),
 ( 1.000000000000000000, 0.7071067811865475727, 1.000000000000000000),
 ( 1.000000000000000000, 0.7071067811865475727, 1.000000000000000000) ) ) 
 REPRESENTATION_ITEM ( '' )  SURFACE ( )  );
#4485 = CARTESIAN_POINT ( 'NONE',  ( -52.59034431212841554, 9.999999999999998224, -168.6389827469478178 ) ) ;
#4486 = CARTESIAN_POINT ( 'NONE',  ( -3.249999999999999556, 1.750000000000000222, -3.500000000000000000 ) ) ;
#4487 = ORIENTED_EDGE ( 'NONE', *, *, #5053, .T. ) ;
#4488 = EDGE_CURVE ( 'NONE', #14756, #6134, #11001, .T. ) ;
#4489 = CARTESIAN_POINT ( 'NONE',  ( 38.25296960060453699, 0.000000000000000000, 42.65758570601131794 ) ) ;
#4490 = CARTESIAN_POINT ( 'NONE',  ( -25.44041662983336849, 3.773872472838732506, -208.9707249988738340 ) ) ;
#4491 = CARTESIAN_POINT ( 'NONE',  ( 6.146471803482498331, 12.22506747196939614, 4.769516544308691763 ) ) ;
#4492 = EDGE_CURVE ( 'NONE', #1124, #9716, #416, .T. ) ;
#4493 = CARTESIAN_POINT ( 'NONE',  ( -9.721966606379332632, 5.000000000000002665, -116.3614657639789414 ) ) ;
#4494 = CARTESIAN_POINT ( 'NONE',  ( 0.000000000000000000, 13.50000000000000355, -0.2500000000000002220 ) ) ;
#4495 = APPROVAL_PERSON_ORGANIZATION ( #6939, #11527, #996 ) ;
#4496 = CARTESIAN_POINT ( 'NONE',  ( 0.000000000000000000, 2.500000000000000000, 0.2500000000000002220 ) ) ;
#4497 = DIRECTION ( 'NONE',  ( 0.000000000000000000, -0.9314983497198060514, 0.3637455490714327500 ) ) ;
#4498 = CARTESIAN_POINT ( 'NONE',  ( -6.525249091262845802, 11.54687804473151758, -124.9828182402523851 ) ) ;
#4499 = CARTESIAN_POINT ( 'NONE',  ( 3.890350893699055845, 0.000000000000000000, -1.782295516753892972 ) ) ;
#4500 = CC_DESIGN_PERSON_AND_ORGANIZATION_ASSIGNMENT ( #12017, #4838, ( #12090 ) ) ;
#4501 = CARTESIAN_POINT ( 'NONE',  ( 4.200501518084891472, 13.70058811643232843, 3.183963981513004970 ) ) ;
#4502 = CARTESIAN_POINT ( 'NONE',  ( 3.249999999999999556, 8.750000000000000000, -3.500000000000000000 ) ) ;
#4503 = CARTESIAN_POINT ( 'NONE',  ( -1.500000000000000000, 5.000000000000000000, 0.2500000000000002220 ) ) ;
#4504 = LOCAL_TIME ( 12, 28, 20.00000000000000000, #7239 ) ;
#4505 = VERTEX_POINT ( 'NONE', #2887 ) ;
#4506 = ORIENTED_EDGE ( 'NONE', *, *, #1793, .F. ) ;
#4507 = CARTESIAN_POINT ( 'NONE',  ( -6.345149115697418019, 2.442921369471867893E-15, -181.1746449140297841 ) ) ;
#4508 = CARTESIAN_POINT ( 'NONE',  ( 3.750000000000000000, 3.750000000000000000, -3.500000000000000444 ) ) ;
#4509 = CARTESIAN_POINT ( 'NONE',  ( -3.980102097228897738E-16, 15.00000000000000178, -6.749999999999999112 ) ) ;
#4510 = CARTESIAN_POINT ( 'NONE',  ( 3.235167919087375221, 15.00000000000000000, -114.6791120453254962 ) ) ;
#4511 = ORIENTED_EDGE ( 'NONE', *, *, #8094, .T. ) ;
#4512 = EDGE_CURVE ( 'NONE', #7762, #1027, #9137, .T. ) ;
#4513 = VECTOR ( 'NONE', #2343, 1000.000000000000114 ) ;
#4514 = CARTESIAN_POINT ( 'NONE',  ( -3.249999999999999556, 14.31250000000000000, -4.846194077712557835 ) ) ;
#4515 = EDGE_CURVE ( 'NONE', #13423, #9221, #7516, .T. ) ;
#4516 = ADVANCED_FACE ( 'NONE', ( #3895 ), #9404, .T. ) ;
#4517 = CARTESIAN_POINT ( 'NONE',  ( -55.30796743861389331, 14.99999999999543476, -150.1894123920446305 ) ) ;
#4518 = CARTESIAN_POINT ( 'NONE',  ( -9.240119717569001523, 10.34875921372550955, -104.6630069174426154 ) ) ;
#4519 = APPROVAL ( #15084, 'UNSPECIFIED' ) ;
#4520 = CARTESIAN_POINT ( 'NONE',  ( -3.249999999999999556, 2.250000000000000444, -3.499999999999999556 ) ) ;
#4521 = DATE_AND_TIME ( #5888, #12598 ) ;
#4522 = FACE_OUTER_BOUND ( 'NONE', #1962, .T. ) ;
#4523 = LINE ( 'NONE', #962, #14836 ) ;
#4524 = ORIENTED_EDGE ( 'NONE', *, *, #14346, .T. ) ;
#4525 = AXIS2_PLACEMENT_3D ( 'NONE', #846, #6857, #13753 ) ;
#4526 = CARTESIAN_POINT ( 'NONE',  ( 25.85064958816917624, 2.055286875431564297, -138.3708915003257971 ) ) ;
#4527 = CARTESIAN_POINT ( 'NONE',  ( -3.249999999999999556, 9.187500000000000000, -2.153805922287440833 ) ) ;
#4528 = ORIENTED_EDGE ( 'NONE', *, *, #10366, .T. ) ;
#4529 = ORIENTED_EDGE ( 'NONE', *, *, #10907, .T. ) ;
#4530 = CARTESIAN_POINT ( 'NONE',  ( -3.750000000000000000, 11.68749999999999822, -1.946699141100893149 ) ) ;
#4531 = DIRECTION ( 'NONE',  ( -0.02181900108494707127, -0.000000000000000000, 0.9997619372588931741 ) ) ;
#4532 = CARTESIAN_POINT ( 'NONE',  ( 2.651650429449552870, 2.125000000000000000, -6.151650429449555091 ) ) ;
#4533 = CARTESIAN_POINT ( 'NONE',  ( 3.249999999999999556, 7.250000000000001776, -3.500000000000000000 ) ) ;
#4534 = ORIENTED_EDGE ( 'NONE', *, *, #8545, .F. ) ;
#4535 = CARTESIAN_POINT ( 'NONE',  ( -9.385448347264267355, 9.999999999999998224, -115.3551636530117150 ) ) ;
#4536 = CARTESIAN_POINT ( 'NONE',  ( -3.249999999999999556, 2.250000000000000444, -3.499999999999999556 ) ) ;
#4537 = ADVANCED_FACE ( 'NONE', ( #8594 ), #13556, .F. ) ;
#4538 = APPROVAL ( #5910, 'UNSPECIFIED' ) ;
#4539 = CARTESIAN_POINT ( 'NONE',  ( -3.750000000000000000, 6.250000000000000000, -3.499999999999999112 ) ) ;
#4540 = AXIS2_PLACEMENT_3D ( 'NONE', #3942, #8644, #11199 ) ;
#4541 = AXIS2_PLACEMENT_3D ( 'NONE', #1273, #41, #11632 ) ;
#4542 = DIRECTION ( 'NONE',  ( 0.000000000000000000, 0.000000000000000000, 1.000000000000000000 ) ) ;
#4543 = CARTESIAN_POINT ( 'NONE',  ( -0.8977508794915173285, -8.673617379884037444E-16, -125.7548904922300181 ) ) ;
#4544 = CALENDAR_DATE ( 2026, 8, 10 ) ;
#4545 = CARTESIAN_POINT ( 'NONE',  ( 26.28048204801264731, 0.000000000000000000, 69.48733826436532013 ) ) ;
#4546 = ORIENTED_EDGE ( 'NONE', *, *, #12925, .T. ) ;
#4547 = VECTOR ( 'NONE', #13299, 1000.000000000000000 ) ;
#4548 = VECTOR ( 'NONE', #789, 1000.000000000000000 ) ;
#4549 = CARTESIAN_POINT ( 'NONE',  ( -1.346194077712558945, 5.562500000000000000, -0.2500000000000002220 ) ) ;
#4550 = DIRECTION ( 'NONE',  ( -0.000000000000000000, 1.000000000000000000, -0.000000000000000000 ) ) ;
#4551 = CARTESIAN_POINT ( 'NONE',  ( 3.749999999999998668, 9.187500000000001776, -5.053300858899108405 ) ) ;
#4552 = CARTESIAN_POINT ( 'NONE',  ( 3.750000000000000000, 11.75000000000000000, -3.500000000000000444 ) ) ;
#4553 = CARTESIAN_POINT ( 'NONE',  ( -67.58587069055120367, 13.53642980795543593, -200.6028043760882724 ) ) ;
#4554 = CARTESIAN_POINT ( 'NONE',  ( -1.871645213090456616, 5.000000000000011546, -133.9039370687633834 ) ) ;
#4555 = CARTESIAN_POINT ( 'NONE',  ( -3.249999999999999556, -0.2499999999999998890, -3.500000000000000000 ) ) ;
#4556 = AXIS2_PLACEMENT_3D ( 'NONE', #494, #5212, #13493 ) ;
#4557 = CARTESIAN_POINT ( 'NONE',  ( -10.46704385831657902, 0.000000000000000000, -128.9524512386204549 ) ) ;
#4558 = APPROVAL_ROLE ( '' ) ;
#4559 = LINE ( 'NONE', #4630, #12217 ) ;
#4560 = VERTEX_POINT ( 'NONE', #12382 ) ;
#4561 = CARTESIAN_POINT ( 'NONE',  ( 8.783361249427379391, 3.744510042675810446, 2.765904461544427928 ) ) ;
#4562 = CARTESIAN_POINT ( 'NONE',  ( -2.298097038856278918, 3.375000000000000000, -5.798097038856277585 ) ) ;
#4563 = CARTESIAN_POINT ( 'NONE',  ( -56.64898049662669877, 15.00000000000794032, -176.0284089207902980 ) ) ;
#4564 = CARTESIAN_POINT ( 'NONE',  ( -2.298097038856279362, 2.875000000000000000, -5.798097038856278473 ) ) ;
#4565 = VERTEX_POINT ( 'NONE', #12155 ) ;
#4566 = CARTESIAN_POINT ( 'NONE',  ( 1.396221076823685792, -2.558678233169546790, -1.000000000000001332 ) ) ;
#4567 = CARTESIAN_POINT ( 'NONE',  ( -19.94423925787078389, 15.00000000000000000, -150.2885610952392881 ) ) ;
#4568 = CARTESIAN_POINT ( 'NONE',  ( 6.257758434032409944, 14.35016516265838682, 2.760946016300349637 ) ) ;
#4569 = CARTESIAN_POINT ( 'NONE',  ( -2.027137927705678688, 3.249798772148220769E-12, -107.0032022125478761 ) ) ;
#4570 = CARTESIAN_POINT ( 'NONE',  ( 2.298097038856278029, 11.12500000000000178, -5.798097038856279362 ) ) ;
#4571 = CARTESIAN_POINT ( 'NONE',  ( 0.3766621274091721538, 0.3292059843107342232, -7.146945437571387671 ) ) ;
#4572 = CARTESIAN_POINT ( 'NONE',  ( 3.750000000000000000, 1.312500000000000444, -1.946699141100892705 ) ) ;
#4573 = CYLINDRICAL_SURFACE ( 'NONE', #4778, 7.000000000000016875 ) ;
#4574 = EDGE_CURVE ( 'NONE', #4119, #9480, #14334, .T. ) ;
#4575 = CARTESIAN_POINT ( 'NONE',  ( -5.538366777589915912, 13.14664760303528901, -125.0671679570068164 ) ) ;
#4576 =( BOUNDED_SURFACE ( )  B_SPLINE_SURFACE ( 3, 1, ( 
 ( #3262, #14886 ),
 ( #12850, #2111 ),
 ( #10152, #4283 ),
 ( #6816, #8989 ) ),
 .UNSPECIFIED., .F., .F., .F. ) 
 B_SPLINE_SURFACE_WITH_KNOTS ( ( 4, 4 ),
 ( 2, 2 ),
 ( 0.000000000000000000, 1.000000000000000000 ),
 ( 0.000000000000000000, 1.000000000000000000 ),
 .UNSPECIFIED. ) 
 GEOMETRIC_REPRESENTATION_ITEM ( )  RATIONAL_B_SPLINE_SURFACE ( (
 ( 1.000000000000000000, 1.000000000000000000),
 ( 0.8750842653720394271, 0.8750842653720394271),
 ( 0.8750842653720394271, 0.8750842653720394271),
 ( 1.000000000000000000, 1.000000000000000000) ) ) 
 REPRESENTATION_ITEM ( '' )  SURFACE ( )  );
#4577 = CARTESIAN_POINT ( 'NONE',  ( -25.82983890416511841, 5.000000000000000000, -142.4527639562402328 ) ) ;
#4578 = EDGE_CURVE ( 'NONE', #12491, #2651, #7747, .T. ) ;
#4579 = CARTESIAN_POINT ( 'NONE',  ( -5.068140779129265638, 2.100000000000000089, 4.126857918875922238 ) ) ;
#4580 = CARTESIAN_POINT ( 'NONE',  ( 0.000000000000000000, 13.00000000000000178, -0.2500000000000002220 ) ) ;
#4581 = DIRECTION ( 'NONE',  ( 0.000000000000000000, -0.000000000000000000, -1.000000000000000000 ) ) ;
#4582 = CARTESIAN_POINT ( 'NONE',  ( -17.32624372123753886, 15.00000000000000000, -122.3796757791585321 ) ) ;
#4583 = EDGE_LOOP ( 'NONE', ( #12957, #7204, #4066, #2528, #10336, #6565, #1287, #11922 ) ) ;
#4584 = ORIENTED_EDGE ( 'NONE', *, *, #3291, .F. ) ;
#4585 = CARTESIAN_POINT ( 'NONE',  ( 8.820757121451897831, 15.00000000000000000, -106.4638369497514105 ) ) ;
#4586 = CARTESIAN_POINT ( 'NONE',  ( -1.553300858899107295, 5.437500000000002665, -7.250000000000000000 ) ) ;
#4587 = CARTESIAN_POINT ( 'NONE',  ( -3.249999999999999112, 13.81250000000000178, -4.846194077712558723 ) ) ;
#4588 = CARTESIAN_POINT ( 'NONE',  ( -8.602511404923770755, -2.262486257093532419E-12, -105.7492080830174359 ) ) ;
#4589 = ORIENTED_EDGE ( 'NONE', *, *, #412, .T. ) ;
#4590 = CARTESIAN_POINT ( 'NONE',  ( -3.249999999999999556, 0.7499999999999998890, -3.500000000000000000 ) ) ;
#4591 = CC_DESIGN_PERSON_AND_ORGANIZATION_ASSIGNMENT ( #211, #911, ( #8443 ) ) ;
#4592 = FACE_OUTER_BOUND ( 'NONE', #12594, .T. ) ;
#4593 = DIRECTION ( 'NONE',  ( 0.000000000000000000, 0.000000000000000000, 1.000000000000000000 ) ) ;
#4594 = CARTESIAN_POINT ( 'NONE',  ( -3.980102097228897245E-16, 4.500000000000000888, -6.749999999999999112 ) ) ;
#4595 = APPROVAL_DATE_TIME ( #4666, #2152 ) ;
#4596 = DIRECTION ( 'NONE',  ( -0.000000000000000000, -1.000000000000000000, 0.000000000000000000 ) ) ;
#4597 = DIRECTION ( 'NONE',  ( 0.9961255586397056438, -0.000000000000000000, -0.08794243244722428632 ) ) ;
#4598 = ORIENTED_EDGE ( 'NONE', *, *, #3387, .F. ) ;
#4599 = EDGE_CURVE ( 'NONE', #5461, #3224, #8152, .T. ) ;
#4600 = CARTESIAN_POINT ( 'NONE',  ( 0.2499999999999999445, 4.500000000000000888, 0.2500000000000002220 ) ) ;
#4601 = CARTESIAN_POINT ( 'NONE',  ( -3.249999999999999556, 12.31250000000000000, -4.846194077712557835 ) ) ;
#4602 = ORIENTED_EDGE ( 'NONE', *, *, #12990, .T. ) ;
#4603 = ORIENTED_EDGE ( 'NONE', *, *, #4515, .T. ) ;
#4604 = CARTESIAN_POINT ( 'NONE',  ( -1.553300858899107073, 7.937500000000001776, -7.249999999999999112 ) ) ;
#4605 = CARTESIAN_POINT ( 'NONE',  ( -20.05675593593863582, 9.999999999999998224, -128.8251628084967706 ) ) ;
#4606 = CARTESIAN_POINT ( 'NONE',  ( 3.749999999999999112, 7.187500000000000888, -5.053300858899108405 ) ) ;
#4607 = CARTESIAN_POINT ( 'NONE',  ( 3.249999999999998224, 8.187500000000000000, -4.846194077712561388 ) ) ;
#4608 = ORIENTED_EDGE ( 'NONE', *, *, #14188, .T. ) ;
#4609 = CARTESIAN_POINT ( 'NONE',  ( 6.208467851984790009, 13.77618473890310291, 3.570604971030389319 ) ) ;
#4610 = CARTESIAN_POINT ( 'NONE',  ( -3.980102097228897245E-16, 1.500000000000000000, -6.749999999999999112 ) ) ;
#4611 = CARTESIAN_POINT ( 'NONE',  ( 3.749999999999999112, 5.812500000000000000, -1.946699141100892039 ) ) ;
#4612 = CARTESIAN_POINT ( 'NONE',  ( -25.60675101229562500, 1.982032305613783407, -207.4180151373524268 ) ) ;
#4613 = CARTESIAN_POINT ( 'NONE',  ( -4.975935430107378821, 0.000000000000000000, -1.000000000000001332 ) ) ;
#4614 = CARTESIAN_POINT ( 'NONE',  ( 6.012727666029630491, 15.00000000000000000, -116.3088615718675385 ) ) ;
#4615 = PERSON_AND_ORGANIZATION_ROLE ( 'design_owner' ) ;
#4616 = CARTESIAN_POINT ( 'NONE',  ( -14.41690554581313854, 7.499999999999991118, -89.38856786110081032 ) ) ;
#4617 = FACE_OUTER_BOUND ( 'NONE', #11386, .T. ) ;
#4618 = EDGE_CURVE ( 'NONE', #13258, #3495, #1741, .T. ) ;
#4619 = EDGE_LOOP ( 'NONE', ( #11646, #3437, #4754, #7557 ) ) ;
#4620 = CARTESIAN_POINT ( 'NONE',  ( -1.346194077712558945, 8.562500000000001776, -0.2500000000000002220 ) ) ;
#4621 = CARTESIAN_POINT ( 'NONE',  ( 9.884674853941351813, 8.773889247172311556, -40.63426294266372452 ) ) ;
#4622 = CARTESIAN_POINT ( 'NONE',  ( -4.592425496802573972E-16, 11.00000000000000178, -7.250000000000000000 ) ) ;
#4623 = AXIS2_PLACEMENT_3D ( 'NONE', #7199, #14499, #341 ) ;
#4624 = CARTESIAN_POINT ( 'NONE',  ( -2.651650429449553314, 12.37500000000000000, -6.151650429449552426 ) ) ;
#4625 = CARTESIAN_POINT ( 'NONE',  ( -66.21231308551345762, 14.86702644051741551, -190.0915466865270673 ) ) ;
#4626 = CARTESIAN_POINT ( 'NONE',  ( -8.628312869877936109, 5.000000000000000888, -120.2932534013991130 ) ) ;
#4627 = CARTESIAN_POINT ( 'NONE',  ( -2.298097038856278029, -0.3749999999999998890, -1.201902961143720638 ) ) ;
#4628 = CARTESIAN_POINT ( 'NONE',  ( -3.725055588901181824, 4.336808689942017243E-16, -108.1536978458372147 ) ) ;
#4629 = PERSON_AND_ORGANIZATION_ROLE ( 'design_owner' ) ;
#4630 = CARTESIAN_POINT ( 'NONE',  ( 26.28048204801264731, 0.000000000000000000, 69.48733826436532013 ) ) ;
#4631 = B_SPLINE_CURVE_WITH_KNOTS ( 'NONE', 3,
 ( #8912, #2110, #6746, #6815, #3115, #7675, #1887, #878, #3261, #4207, #7828, #15033, #12542, #806, #1953, #5581 ),
 .UNSPECIFIED., .F., .F.,
 ( 4, 2, 2, 2, 2, 2, 2, 4 ),
 ( 0.000000000000000000, 0.0009849038691403968863, 0.001969807738280793773, 0.003939615476561587545, 0.004924519345701984865, 0.005909423214842381318, 0.006894327083982777771, 0.007879230953123175091 ),
 .UNSPECIFIED. ) ;
#4632 = ORIENTED_EDGE ( 'NONE', *, *, #11230, .F. ) ;
#4633 = CARTESIAN_POINT ( 'NONE',  ( -44.21823081166466096, 9.999999999999998224, -145.3603131190973272 ) ) ;
#4634 = CARTESIAN_POINT ( 'NONE',  ( 2.298097038856278473, 4.625000000000000000, -5.798097038856279362 ) ) ;
#4635 = CARTESIAN_POINT ( 'NONE',  ( -52.20743557207289598, 9.999999999999998224, -168.0633964595267571 ) ) ;
#4636 = CARTESIAN_POINT ( 'NONE',  ( 3.249999999999998224, 8.187500000000000000, -4.846194077712561388 ) ) ;
#4637 = ORIENTED_EDGE ( 'NONE', *, *, #1168, .T. ) ;
#4638 = CARTESIAN_POINT ( 'NONE',  ( 4.921100845785776556, 4.999999999999999112, -108.2352075023247409 ) ) ;
#4639 = CARTESIAN_POINT ( 'NONE',  ( -25.48272420619116474, 0.09695822977917610552, -201.3338006394713204 ) ) ;
#4640 = CARTESIAN_POINT ( 'NONE',  ( 8.987202726980132894, 12.50000000278589596, 0.4885395538092229262 ) ) ;
#4641 = DIRECTION ( 'NONE',  ( 0.4321074940959399036, -0.8090169943749466741, 0.3984653264195704980 ) ) ;
#4642 = CARTESIAN_POINT ( 'NONE',  ( -1.346194077712558945, 13.56250000000000000, -0.2500000000000002220 ) ) ;
#4643 = CARTESIAN_POINT ( 'NONE',  ( -0.2500000000000000555, 5.000000000000000000, 1.500000000000000222 ) ) ;
#4644 = CARTESIAN_POINT ( 'NONE',  ( -2.651650429449552870, 2.625000000000000000, -0.8483495705504463524 ) ) ;
#4645 = PLANE ( 'NONE',  #2066 ) ;
#4646 = DIRECTION ( 'NONE',  ( 0.08794243244723003172, 0.000000000000000000, 0.9961255586397049777 ) ) ;
#4647 = CARTESIAN_POINT ( 'NONE',  ( 25.31442990777252433, 1.743671408225548891, -137.3942114566015675 ) ) ;
#4648 = CARTESIAN_POINT ( 'NONE',  ( -5.542419796536699472, 0.000000000000000000, 11.20594165676177134 ) ) ;
#4649 = CARTESIAN_POINT ( 'NONE',  ( -1.346194077712559389, 14.06249999999999822, -0.2500000000000002220 ) ) ;
#4650 = CARTESIAN_POINT ( 'NONE',  ( -7.171502477872234493, 14.01677234745007183, -104.0350480920882319 ) ) ;
#4651 = DIRECTION ( 'NONE',  ( 0.000000000000000000, 0.000000000000000000, 1.000000000000000000 ) ) ;
#4652 = ORIENTED_EDGE ( 'NONE', *, *, #7305, .F. ) ;
#4653 = ORIENTED_EDGE ( 'NONE', *, *, #6584, .F. ) ;
#4654 = CARTESIAN_POINT ( 'NONE',  ( -5.617373260391812728, 0.000000000000000000, -174.7795128502804403 ) ) ;
#4655 = CARTESIAN_POINT ( 'NONE',  ( 2.651650429449552870, 4.625000000000000000, -6.151650429449554203 ) ) ;
#4656 = CARTESIAN_POINT ( 'NONE',  ( -2.651650429449552870, 5.625000000000000000, -0.8483495705504467965 ) ) ;
#4657 = DIRECTION ( 'NONE',  ( 0.000000000000000000, 0.000000000000000000, -1.000000000000000000 ) ) ;
#4658 = VERTEX_POINT ( 'NONE', #11528 ) ;
#4659 = CARTESIAN_POINT ( 'NONE',  ( -3.249999999999999112, 0.6875000000000000000, -2.153805922287440833 ) ) ;
#4660 = CIRCLE ( 'NONE', #4418, 4.999999999999995559 ) ;
#4661 = B_SPLINE_CURVE_WITH_KNOTS ( 'NONE', 3,
 ( #5147, #12480, #7461, #14594, #1822, #12176, #1595, #3996, #9859, #6611, #12401, #11090 ),
 .UNSPECIFIED., .F., .F.,
 ( 4, 2, 2, 2, 2, 4 ),
 ( 1.734723475976807094E-18, 0.001027444902010466940, 0.002054889804020932145, 0.003082334706031397351, 0.003596057157036637326, 0.004109779608041877301 ),
 .UNSPECIFIED. ) ;
#4662 = EDGE_CURVE ( 'NONE', #602, #1534, #10625, .T. ) ;
#4663 = CARTESIAN_POINT ( 'NONE',  ( -52.65879960168029328, 9.999999999999998224, -146.8206079633650063 ) ) ;
#4664 = CARTESIAN_POINT ( 'NONE',  ( 16.10717976051956413, 8.673617379884033500E-16, -135.3045475799466999 ) ) ;
#4665 = CARTESIAN_POINT ( 'NONE',  ( -1.346194077712559389, 2.062500000000000000, -0.2500000000000002220 ) ) ;
#4666 = DATE_AND_TIME ( #5746, #13084 ) ;
#4667 = CARTESIAN_POINT ( 'NONE',  ( -0.2500000000000000555, 4.500000000000000888, 0.2500000000000002220 ) ) ;
#4668 = DIRECTION ( 'NONE',  ( -0.000000000000000000, -1.000000000000000000, -0.000000000000000000 ) ) ;
#4669 = ORIENTED_EDGE ( 'NONE', *, *, #13666, .T. ) ;
#4670 = CARTESIAN_POINT ( 'NONE',  ( 2.689713740728195024, -1.628626824712336996, -1.000000000000001332 ) ) ;
#4671 = CARTESIAN_POINT ( 'NONE',  ( 3.249999999999998668, 13.68750000000000000, -4.846194077712560500 ) ) ;
#4672 = ORIENTED_EDGE ( 'NONE', *, *, #14788, .F. ) ;
#4673 = ORIENTED_EDGE ( 'NONE', *, *, #6874, .T. ) ;
#4674 = CARTESIAN_POINT ( 'NONE',  ( -5.836568743579779728, 2.331468351712828340E-16, 17.25548782215969368 ) ) ;
#4675 = CARTESIAN_POINT ( 'NONE',  ( -3.750000000000000000, 4.687500000000000888, -1.946699141100893149 ) ) ;
#4676 = CARTESIAN_POINT ( 'NONE',  ( 0.000000000000000000, 5.500000000000000888, -0.2500000000000002220 ) ) ;
#4677 = EDGE_LOOP ( 'NONE', ( #5439, #12967, #2617, #3192 ) ) ;
#4678 = CARTESIAN_POINT ( 'NONE',  ( 6.134605308603925167, 11.61845493593924417, 5.022560416558600416 ) ) ;
#4679 = CARTESIAN_POINT ( 'NONE',  ( -1.346194077712559389, 4.437500000000000888, -6.749999999999999112 ) ) ;
#4680 = EDGE_CURVE ( 'NONE', #7347, #1934, #7406, .T. ) ;
#4681 = CARTESIAN_POINT ( 'NONE',  ( -1.553300858899107295, 10.43750000000000000, -7.250000000000000000 ) ) ;
#4682 = CARTESIAN_POINT ( 'NONE',  ( -25.62274278772851943, 0.2453806450821310603, -202.6740962663072025 ) ) ;
#4683 = CARTESIAN_POINT ( 'NONE',  ( 6.770579566034210295, -2.743867526398025447, -34.56909192082981974 ) ) ;
#4684 = APPROVAL_DATE_TIME ( #11717, #668 ) ;
#4685 = CARTESIAN_POINT ( 'NONE',  ( 39.42664711868611960, 1.750000000000000000, 42.16864325401552804 ) ) ;
#4686 = APPROVAL_PERSON_ORGANIZATION ( #3200, #4690, #4371 ) ;
#4687 = EDGE_LOOP ( 'NONE', ( #7061, #10452 ) ) ;
#4688 = AXIS2_PLACEMENT_3D ( 'NONE', #15260, #13070, #4651 ) ;
#4689 = CARTESIAN_POINT ( 'NONE',  ( 2.298097038856279362, 7.375000000000000000, -1.201902961143720860 ) ) ;
#4690 = APPROVAL ( #9003, 'UNSPECIFIED' ) ;
#4691 = CARTESIAN_POINT ( 'NONE',  ( 8.131300352726233527, 2.490287375297125294, -39.89901737624450107 ) ) ;
#4692 = ADVANCED_FACE ( 'NONE', ( #2178 ), #4351, .T. ) ;
#4693 = CARTESIAN_POINT ( 'NONE',  ( -1.553300858899107073, 11.93750000000000178, -7.249999999999999112 ) ) ;
#4694 = EDGE_CURVE ( 'NONE', #5312, #13029, #7660, .T. ) ;
#4695 = CARTESIAN_POINT ( 'NONE',  ( -6.790153584124040798, 13.40945642053105225, -124.9643354754709748 ) ) ;
#4696 = EDGE_CURVE ( 'NONE', #6539, #882, #6811, .T. ) ;
#4697 = LOCAL_TIME ( 12, 28, 20.00000000000000000, #15274 ) ;
#4698 = CARTESIAN_POINT ( 'NONE',  ( -66.76779559092599925, 14.71819778747807206, -193.1373159669256836 ) ) ;
#4699 = DIRECTION ( 'NONE',  ( 0.9982196940171965682, 0.000000000000000000, -0.05964429961207244613 ) ) ;
#4700 = CARTESIAN_POINT ( 'NONE',  ( 3.750000000000000000, 12.31250000000000178, -1.946699141100892705 ) ) ;
#4701 = CARTESIAN_POINT ( 'NONE',  ( 1.243260443319662123, 4.000000000000000000, -139.4020581015306846 ) ) ;
#4702 = TOROIDAL_SURFACE ( 'NONE', #7143, 8.000000000000000000, 5.000000000000000000 ) ;
#4703 = PERSON_AND_ORGANIZATION ( #3176, #3020 ) ;
#4704 = VECTOR ( 'NONE', #7157, 1000.000000000000000 ) ;
#4705 = CARTESIAN_POINT ( 'NONE',  ( -2.298097038856278918, 14.37500000000000000, -5.798097038856277585 ) ) ;
#4706 = CARTESIAN_POINT ( 'NONE',  ( 9.044950117654433797, 6.000000000000000000, -137.9826476090360643 ) ) ;
#4707 = ORIENTED_EDGE ( 'NONE', *, *, #3062, .T. ) ;
#4708 = CARTESIAN_POINT ( 'NONE',  ( -22.51849958723530776, 8.673617379884035472E-16, -204.9231702217275028 ) ) ;
#4709 = CARTESIAN_POINT ( 'NONE',  ( 3.249999999999999112, 3.812500000000000000, -2.153805922287439945 ) ) ;
#4710 = CARTESIAN_POINT ( 'NONE',  ( -63.24671589544669814, 9.999999999999998224, -204.0178512890850868 ) ) ;
#4711 = AXIS2_PLACEMENT_3D ( 'NONE', #11605, #10449, #10591 ) ;
#4712 = CARTESIAN_POINT ( 'NONE',  ( -3.249999999999999112, 6.687500000000000888, -2.153805922287440833 ) ) ;
#4713 = ORIENTED_EDGE ( 'NONE', *, *, #1256, .F. ) ;
#4714 = CARTESIAN_POINT ( 'NONE',  ( -5.187227155321425975, 14.99999999999878142, -114.5705604395851083 ) ) ;
#4715 = AXIS2_PLACEMENT_3D ( 'NONE', #14737, #12165, #11158 ) ;
#4716 = AXIS2_PLACEMENT_3D ( 'NONE', #11870, #12254, #11089 ) ;
#4717 = CARTESIAN_POINT ( 'NONE',  ( -8.205916711996726676, 7.499999999999991118, -92.94857034792688921 ) ) ;
#4718 = CARTESIAN_POINT ( 'NONE',  ( -17.32624372123753886, 15.00000000000000000, -122.3796757791585321 ) ) ;
#4719 = CARTESIAN_POINT ( 'NONE',  ( 0.000000000000000000, 2.000000000000000000, -0.2500000000000002220 ) ) ;
#4720 = CARTESIAN_POINT ( 'NONE',  ( -2.298097038856278029, 11.62500000000000000, -1.201902961143720638 ) ) ;
#4721 = CARTESIAN_POINT ( 'NONE',  ( -0.1251224477187976580, 0.2925544614197072568, -7.146945437571384119 ) ) ;
#4722 = CARTESIAN_POINT ( 'NONE',  ( 0.000000000000000000, 3.500000000000000000, 0.2500000000000002220 ) ) ;
#4723 = CARTESIAN_POINT ( 'NONE',  ( 0.5065669725921494448, 10.41780148816173579, 5.737893171667577619 ) ) ;
#4724 = AXIS2_PLACEMENT_3D ( 'NONE', #9002, #6536, #2047 ) ;
#4725 = CARTESIAN_POINT ( 'NONE',  ( 5.844703153020811115, 9.999999999999998224, -103.2023327213425432 ) ) ;
#4726 = CARTESIAN_POINT ( 'NONE',  ( 25.05271902006223783, 1.500039406472921222, -137.4898610820562510 ) ) ;
#4727 = CARTESIAN_POINT ( 'NONE',  ( 5.873062173554511212, 2.100000000000850964, 52.35081790185157757 ) ) ;
#4728 = CARTESIAN_POINT ( 'NONE',  ( -3.249999999999999556, 13.18749999999999822, -2.153805922287440833 ) ) ;
#4729 = DIRECTION ( 'NONE',  ( 0.9989498407774402011, -0.000000000000000000, 0.04581719776161457397 ) ) ;
#4730 = DIRECTION ( 'NONE',  ( -0.9961255586397050887, 0.000000000000000000, 0.08794243244723005948 ) ) ;
#4731 = ORIENTED_EDGE ( 'NONE', *, *, #1491, .F. ) ;
#4732 = VERTEX_POINT ( 'NONE', #3335 ) ;
#4733 = CARTESIAN_POINT ( 'NONE',  ( -5.191659272726472985, -2.650598460978561364E-13, -112.0623128200408303 ) ) ;
#4734 = CARTESIAN_POINT ( 'NONE',  ( 6.162973360166584591, 8.673617379884035472E-16, -165.1928244853837384 ) ) ;
#4735 = CARTESIAN_POINT ( 'NONE',  ( 3.749999999999999112, 3.812500000000000000, -1.946699141100892039 ) ) ;
#4736 = CARTESIAN_POINT ( 'NONE',  ( 1.553300858899105963, 5.062500000000000000, -7.249999999999999112 ) ) ;
#4737 = VERTEX_POINT ( 'NONE', #14880 ) ;
#4738 = CARTESIAN_POINT ( 'NONE',  ( -6.679542461294181166, 0.5769591943446209514, -116.5285319886242803 ) ) ;
#4739 = CARTESIAN_POINT ( 'NONE',  ( -2.298097038856278918, 13.37500000000000000, -5.798097038856277585 ) ) ;
#4740 = FACE_OUTER_BOUND ( 'NONE', #1661, .T. ) ;
#4741 = FACE_OUTER_BOUND ( 'NONE', #9613, .T. ) ;
#4742 = CARTESIAN_POINT ( 'NONE',  ( -3.249999999999999556, 3.250000000000000444, -3.499999999999999556 ) ) ;
#4743 = CALENDAR_DATE ( 2026, 8, 10 ) ;
#4744 = APPROVAL_PERSON_ORGANIZATION ( #139, #10863, #9490 ) ;
#4745 = CARTESIAN_POINT ( 'NONE',  ( 10.54086443187302891, 12.49999999999999822, -107.6778029779925276 ) ) ;
#4746 = ORIENTED_EDGE ( 'NONE', *, *, #13250, .F. ) ;
#4747 = CARTESIAN_POINT ( 'NONE',  ( -0.1555714895694204625, 15.00000000000000000, -114.4873493435821246 ) ) ;
#4748 = DIRECTION ( 'NONE',  ( -0.000000000000000000, -1.000000000000000000, -0.000000000000000000 ) ) ;
#4749 = ORIENTED_EDGE ( 'NONE', *, *, #5370, .F. ) ;
#4750 = ORIENTED_EDGE ( 'NONE', *, *, #6495, .T. ) ;
#4751 = CARTESIAN_POINT ( 'NONE',  ( 0.000000000000000000, 0.2006112523677016646, 0.1491815183709511716 ) ) ;
#4752 = CARTESIAN_POINT ( 'NONE',  ( 3.749999999999999556, 6.250000000000000888, -3.500000000000000444 ) ) ;
#4753 = CARTESIAN_POINT ( 'NONE',  ( -2.298097038856278029, 7.625000000000001776, -1.201902961143720638 ) ) ;
#4754 = ORIENTED_EDGE ( 'NONE', *, *, #8197, .T. ) ;
#4755 = CARTESIAN_POINT ( 'NONE',  ( 4.246495378555050770, 14.99999999999999822, -105.2373590921481536 ) ) ;
#4756 =( BOUNDED_SURFACE ( )  B_SPLINE_SURFACE ( 3, 1, ( 
 ( #6377, #4695 ),
 ( #3535, #9935 ),
 ( #9410, #8243 ),
 ( #14671, #4075 ) ),
 .UNSPECIFIED., .F., .F., .F. ) 
 B_SPLINE_SURFACE_WITH_KNOTS ( ( 4, 4 ),
 ( 2, 2 ),
 ( 0.000000000000000000, 1.000000000000000000 ),
 ( 0.000000000000000000, 1.000000000000000000 ),
 .UNSPECIFIED. ) 
 GEOMETRIC_REPRESENTATION_ITEM ( )  RATIONAL_B_SPLINE_SURFACE ( (
 ( 1.000000000000000000, 1.000000000000000000),
 ( 0.9998070924708732932, 0.9998070924708732932),
 ( 0.9998070924708732932, 0.9998070924708732932),
 ( 1.000000000000000000, 1.000000000000000000) ) ) 
 REPRESENTATION_ITEM ( '' )  SURFACE ( )  );
#4757 = CARTESIAN_POINT ( 'NONE',  ( 2.298097038856278473, 4.625000000000000000, -5.798097038856279362 ) ) ;
#4758 = LINE ( 'NONE', #6229, #1992 ) ;
#4759 = CARTESIAN_POINT ( 'NONE',  ( 3.863626520209246795, -4.336808689942017736E-15, -133.2112599781813174 ) ) ;
#4760 = AXIS2_PLACEMENT_3D ( 'NONE', #768, #917, #3080 ) ;
#4761 = CARTESIAN_POINT ( 'NONE',  ( 7.865309076558498091, 15.00000000000000000, -121.7325209303464959 ) ) ;
#4762 = COORDINATED_UNIVERSAL_TIME_OFFSET ( 0, 0, .AHEAD. ) ;
#4763 = DIRECTION ( 'NONE',  ( -0.02181900108494737658, 0.000000000000000000, 0.9997619372588931741 ) ) ;
#4764 = ORIENTED_EDGE ( 'NONE', *, *, #9993, .F. ) ;
#4765 = EDGE_CURVE ( 'NONE', #13794, #12985, #6176, .T. ) ;
#4766 = CARTESIAN_POINT ( 'NONE',  ( -7.194037649453649763, 0.000000000000000000, -45.55632290616381397 ) ) ;
#4767 = AXIS2_PLACEMENT_3D ( 'NONE', #11558, #13896, #2437 ) ;
#4768 = CARTESIAN_POINT ( 'NONE',  ( -1.553300858899107073, 14.93750000000000000, -7.249999999999999112 ) ) ;
#4769 = CARTESIAN_POINT ( 'NONE',  ( 1.114947364559091492, 5.000000000000000888, -139.4079432275549948 ) ) ;
#4770 = CARTESIAN_POINT ( 'NONE',  ( -63.31408601554949911, 11.08167271840351376, -203.3839820180451454 ) ) ;
#4771 = CARTESIAN_POINT ( 'NONE',  ( 29.28282515376967865, 8.773889247172311556, -47.21258073259075871 ) ) ;
#4772 = CARTESIAN_POINT ( 'NONE',  ( 0.000000000000000000, 2.500000000000000000, -0.2500000000000002220 ) ) ;
#4773 = CARTESIAN_POINT ( 'NONE',  ( 6.599362577383862671, 5.362371901635187827E-13, -105.1339869880811477 ) ) ;
#4774 = SHAPE_DEFINITION_REPRESENTATION ( #2643, #12477 ) ;
#4775 = CARTESIAN_POINT ( 'NONE',  ( -31.09209721305613527, 10.00000000000000178, -156.3611406121567597 ) ) ;
#4776 = AXIS2_PLACEMENT_3D ( 'NONE', #13897, #13459, #830 ) ;
#4777 = CARTESIAN_POINT ( 'NONE',  ( 0.2499999999999999445, 5.000000000000000000, 1.500000000000000222 ) ) ;
#4778 = AXIS2_PLACEMENT_3D ( 'NONE', #8267, #9435, #12768 ) ;
#4779 = VERTEX_POINT ( 'NONE', #13936 ) ;
#4780 = EDGE_CURVE ( 'NONE', #1748, #10459, #6334, .T. ) ;
#4781 = CARTESIAN_POINT ( 'NONE',  ( 5.249698980305105955, 0.08115359711835153089, 1.152527031878756159 ) ) ;
#4782 = CARTESIAN_POINT ( 'NONE',  ( -3.249999999999999556, 2.250000000000000444, -3.499999999999999556 ) ) ;
#4783 = EDGE_CURVE ( 'NONE', #11984, #14278, #13325, .T. ) ;
#4784 = CARTESIAN_POINT ( 'NONE',  ( -61.08087366678788754, 9.999999999999998224, -189.6635742862258098 ) ) ;
#4785 = CARTESIAN_POINT ( 'NONE',  ( -3.249999999999999112, 7.812500000000000000, -4.846194077712558723 ) ) ;
#4786 = EDGE_LOOP ( 'NONE', ( #6295, #12878 ) ) ;
#4787 = CARTESIAN_POINT ( 'NONE',  ( -5.114204838963765987, 15.00000000000000000, -113.1151338089720753 ) ) ;
#4788 = UNCERTAINTY_MEASURE_WITH_UNIT (LENGTH_MEASURE( 1.000000000000000082E-05 ), #12712, 'distance_accuracy_value', 'NONE');
#4789 = CARTESIAN_POINT ( 'NONE',  ( -4.924771681124648026, 0.000000000000000000, -137.0932397189673111 ) ) ;
#4790 = CARTESIAN_POINT ( 'NONE',  ( -17.48543850042227277, 15.00000000000000000, -148.4417142955295219 ) ) ;
#4791 = CARTESIAN_POINT ( 'NONE',  ( -1.346194077712559389, 1.062500000000000222, -0.2500000000000002220 ) ) ;
#4792 = CONICAL_SURFACE ( 'NONE', #7764, 0.5000000000000018874, 0.6283185307179600665 ) ;
#4793 = CARTESIAN_POINT ( 'NONE',  ( -1.346194077712558945, 14.56250000000000000, -0.2500000000000002220 ) ) ;
#4794 = CARTESIAN_POINT ( 'NONE',  ( 2.651650429449552870, 4.625000000000000000, -6.151650429449554203 ) ) ;
#4795 = CARTESIAN_POINT ( 'NONE',  ( -1.885039096047290252, 8.673617379884034486E-16, -115.1740262261674843 ) ) ;
#4796 = CARTESIAN_POINT ( 'NONE',  ( 2.651650429449552870, 7.125000000000000888, -6.151650429449555091 ) ) ;
#4797 = CARTESIAN_POINT ( 'NONE',  ( 2.427959467901618318, 14.27811504255466346, 3.380083252597285703 ) ) ;
#4798 = CARTESIAN_POINT ( 'NONE',  ( -20.05675593593860384, 5.000000000000000000, -128.8251628084967138 ) ) ;
#4799 = CARTESIAN_POINT ( 'NONE',  ( -2.141054399116760099, 5.000000000000000888, -102.7251783244459773 ) ) ;
#4800 = CARTESIAN_POINT ( 'NONE',  ( -33.91109452335874153, 15.00000000000000000, -156.1716796081737471 ) ) ;
#4801 = CARTESIAN_POINT ( 'NONE',  ( 1.346194077712560944, 11.93750000000000000, -0.2500000000000010547 ) ) ;
#4802 = AXIS2_PLACEMENT_3D ( 'NONE', #9751, #10818, #9900 ) ;
#4803 = EDGE_CURVE ( 'NONE', #6539, #1674, #2996, .T. ) ;
#4804 = CARTESIAN_POINT ( 'NONE',  ( -9.062504774847164768, 11.34291795009329640, -104.6069155299892088 ) ) ;
#4805 = CARTESIAN_POINT ( 'NONE',  ( 7.353370788960563509, 5.000000000000000888, -111.8370434415688663 ) ) ;
#4806 = ORIENTED_EDGE ( 'NONE', *, *, #13873, .T. ) ;
#4807 = VERTEX_POINT ( 'NONE', #6960 ) ;
#4808 = CARTESIAN_POINT ( 'NONE',  ( -3.296136538559349294, 8.673617379884035472E-16, -117.8031853635174144 ) ) ;
#4809 = LINE ( 'NONE', #9292, #15178 ) ;
#4810 = CARTESIAN_POINT ( 'NONE',  ( 0.000000000000000000, 6.000000000000000000, 0.2500000000000002220 ) ) ;
#4811 = CARTESIAN_POINT ( 'NONE',  ( -2.651650429449552870, 2.625000000000000000, -0.8483495705504467965 ) ) ;
#4812 = CARTESIAN_POINT ( 'NONE',  ( 4.286263797015736595E-16, 5.000000000000000000, 3.500000000000000000 ) ) ;
#4813 = EDGE_LOOP ( 'NONE', ( #12060, #11926 ) ) ;
#4814 = CARTESIAN_POINT ( 'NONE',  ( -4.907357056062867429, 4.733476084610204568E-16, -117.3740583286320884 ) ) ;
#4815 = VECTOR ( 'NONE', #3237, 1000.000000000000000 ) ;
#4816 = CARTESIAN_POINT ( 'NONE',  ( 2.298097038856279362, 4.375000000000000000, -1.201902961143720860 ) ) ;
#4817 = CARTESIAN_POINT ( 'NONE',  ( -47.48189921986828921, 9.999999999999998224, -141.5723758807981483 ) ) ;
#4818 = CARTESIAN_POINT ( 'NONE',  ( 5.292461965453085782, 8.673617379884045333E-16, -106.4530418762676476 ) ) ;
#4819 = CARTESIAN_POINT ( 'NONE',  ( -2.298097038856278473, 3.125000000000000000, -1.201902961143720416 ) ) ;
#4820 = CARTESIAN_POINT ( 'NONE',  ( 11.00064054493036458, 5.000000000000000888, -45.93698146250716263 ) ) ;
#4821 = APPLICATION_CONTEXT ( 'configuration controlled 3d designs of mechanical parts and assemblies' ) ;
#4822 = PERSON_AND_ORGANIZATION_ROLE ( 'classification_officer' ) ;
#4823 = CARTESIAN_POINT ( 'NONE',  ( 10.02128254437710098, 12.49999999999999822, -108.3753986617891343 ) ) ;
#4824 = CARTESIAN_POINT ( 'NONE',  ( 13.25562203920985382, 8.452217897303065567E-13, -125.4200107874790717 ) ) ;
#4825 = ORIENTED_EDGE ( 'NONE', *, *, #648, .F. ) ;
#4826 = CARTESIAN_POINT ( 'NONE',  ( -10.29275726619092524, 0.000000000000000000, -34.56909192082969184 ) ) ;
#4827 = CARTESIAN_POINT ( 'NONE',  ( 17.54434971314415037, 8.749999999999998224, -93.70045838864260190 ) ) ;
#4828 = ORIENTED_EDGE ( 'NONE', *, *, #6609, .F. ) ;
#4829 = ORIENTED_EDGE ( 'NONE', *, *, #14544, .F. ) ;
#4830 = CARTESIAN_POINT ( 'NONE',  ( -0.1255563994759004987, 0.2058028268504220881, 0.1491815183709512549 ) ) ;
#4831 = CARTESIAN_POINT ( 'NONE',  ( -1.553300858899106629, 4.562500000000000000, 0.2500000000000002220 ) ) ;
#4832 = CARTESIAN_POINT ( 'NONE',  ( -1.346194077712559167, 10.93750000000000000, -6.749999999999999112 ) ) ;
#4833 = VERTEX_POINT ( 'NONE', #1095 ) ;
#4834 = CARTESIAN_POINT ( 'NONE',  ( -1.499260709786591317, 9.999999999999998224, -106.0110764665439547 ) ) ;
#4835 = CARTESIAN_POINT ( 'NONE',  ( -3.249999999999999556, 3.250000000000000444, -3.499999999999999556 ) ) ;
#4836 = CARTESIAN_POINT ( 'NONE',  ( -0.3766621274091715987, 0.5000000000000000000, 0.1491815183709511716 ) ) ;
#4837 = CARTESIAN_POINT ( 'NONE',  ( 12.48509882908383872, 2.151549674844647431, -165.6960548549982946 ) ) ;
#4838 = PERSON_AND_ORGANIZATION_ROLE ( 'design_supplier' ) ;
#4839 = DIRECTION ( 'NONE',  ( 0.000000000000000000, 0.000000000000000000, -1.000000000000000000 ) ) ;
#4840 = ORIENTED_EDGE ( 'NONE', *, *, #11678, .F. ) ;
#4841 = DIRECTION ( 'NONE',  ( 0.9961255586397055328, 0.000000000000000000, -0.08794243244722442510 ) ) ;
#4842 = CARTESIAN_POINT ( 'NONE',  ( 1.553300858899109071, 14.43750000000000178, 0.2499999999999989175 ) ) ;
#4843 = CARTESIAN_POINT ( 'NONE',  ( -0.4453226528549816265, -2.225540348348185052E-17, 1.000000000000000000 ) ) ;
#4844 = B_SPLINE_CURVE_WITH_KNOTS ( 'NONE', 3,
 ( #9081, #4444, #11323, #14904, #7919, #12790, #896, #2128, #11624, #6616, #9157, #5670, #6831, #10172, #4373, #9233, #13885, #13732 ),
 .UNSPECIFIED., .F., .F.,
 ( 4, 2, 2, 2, 2, 2, 2, 2, 4 ),
 ( 0.000000000000000000, 0.001051779247122088066, 0.002103558494244176132, 0.003155337741366264197, 0.004207116988488352263, 0.005258896235610439895, 0.006310675482732528395, 0.007362454729854616894, 0.008414233976976704527 ),
 .UNSPECIFIED. ) ;
#4845 = EDGE_CURVE ( 'NONE', #11140, #273, #995, .T. ) ;
#4846 = CARTESIAN_POINT ( 'NONE',  ( -64.37630138765543109, 14.38467296841567666, -209.1382580359011456 ) ) ;
#4847 = CYLINDRICAL_SURFACE ( 'NONE', #6943, 5.000000000000000000 ) ;
#4848 = CARTESIAN_POINT ( 'NONE',  ( 0.000000000000000000, 4.499999999999999112, -0.2500000000000002220 ) ) ;
#4849 = CARTESIAN_POINT ( 'NONE',  ( 9.502539846137461055, 1.145151035800988648, -106.1191373047704190 ) ) ;
#4850 = CALENDAR_DATE ( 2026, 8, 10 ) ;
#4851 = CARTESIAN_POINT ( 'NONE',  ( -33.91109452335874153, 5.000000000000000888, -156.1716796081737471 ) ) ;
#4852 = DIRECTION ( 'NONE',  ( 0.9989498407774362043, 0.000000000000000000, 0.04581719776170026237 ) ) ;
#4853 = ORIENTED_EDGE ( 'NONE', *, *, #4599, .T. ) ;
#4854 = CARTESIAN_POINT ( 'NONE',  ( 7.659091881109533873, 1.637990805669089056, 2.041194214175461763 ) ) ;
#4855 = CARTESIAN_POINT ( 'NONE',  ( 3.249999999999999556, 2.750000000000000000, -3.500000000000000000 ) ) ;
#4856 = CARTESIAN_POINT ( 'NONE',  ( -51.63131585254111400, 9.999999999999996447, -145.6370460379244776 ) ) ;
#4857 = CARTESIAN_POINT ( 'NONE',  ( -2.298097038856278473, 12.12500000000000000, -1.201902961143720416 ) ) ;
#4858 = CARTESIAN_POINT ( 'NONE',  ( -3.249999999999999556, 7.750000000000000888, -3.500000000000000000 ) ) ;
#4859 = ORIENTED_EDGE ( 'NONE', *, *, #7993, .F. ) ;
#4860 = CARTESIAN_POINT ( 'NONE',  ( -5.114204838922819185, 9.999999999999998224, -113.1151338089696452 ) ) ;
#4861 = CARTESIAN_POINT ( 'NONE',  ( 14.22910372453204353, 6.000000000000000000, -126.5134921567817941 ) ) ;
#4862 = CARTESIAN_POINT ( 'NONE',  ( 10.03403318997453297, 14.68779660170870649, -106.1276578890943085 ) ) ;
#4863 = CARTESIAN_POINT ( 'NONE',  ( -17.32624372123753886, 9.999999999999998224, -122.3796757791585321 ) ) ;
#4864 = CARTESIAN_POINT ( 'NONE',  ( 0.000000000000000000, 0.4999999999999999445, 0.2499999999999998057 ) ) ;
#4865 = CARTESIAN_POINT ( 'NONE',  ( -3.750000000000000000, 5.250000000000000000, -3.499999999999999112 ) ) ;
#4866 = LINE ( 'NONE', #2398, #1270 ) ;
#4867 = CARTESIAN_POINT ( 'NONE',  ( -3.749999999999999556, 5.750000000000000888, -3.499999999999999112 ) ) ;
#4868 = CARTESIAN_POINT ( 'NONE',  ( 3.237363708849736454, 14.67058913554037680, 0.2716708463123359563 ) ) ;
#4869 = ADVANCED_FACE ( 'NONE', ( #12921 ), #763, .T. ) ;
#4870 = CARTESIAN_POINT ( 'NONE',  ( -4.254413237569938389, 9.999999999999998224, -48.18981741835666810 ) ) ;
#4871 = CARTESIAN_POINT ( 'NONE',  ( 0.2499999999999999445, 4.500000000000000888, 1.500000000000000222 ) ) ;
#4872 = CARTESIAN_POINT ( 'NONE',  ( -67.58382170693634805, 5.000000000000000000, -204.5178482451963191 ) ) ;
#4873 = CARTESIAN_POINT ( 'NONE',  ( -1.346194077712559389, 13.43749999999999822, -6.749999999999999112 ) ) ;
#4874 = CARTESIAN_POINT ( 'NONE',  ( 8.935548306746154523, 5.000000000000000888, 2.855381328098136162 ) ) ;
#4875 = CARTESIAN_POINT ( 'NONE',  ( -63.30269430573372347, 11.04635765553183724, -203.4099129996182853 ) ) ;
#4876 = VERTEX_POINT ( 'NONE', #2334 ) ;
#4877 = CARTESIAN_POINT ( 'NONE',  ( -1.553300858899107073, 9.937500000000001776, -7.249999999999999112 ) ) ;
#4878 = ORIENTED_EDGE ( 'NONE', *, *, #5073, .F. ) ;
#4879 = CARTESIAN_POINT ( 'NONE',  ( -2.748419769261051471, 4.336808689942017736E-16, -111.4617916898408652 ) ) ;
#4880 = CARTESIAN_POINT ( 'NONE',  ( -10.29275726619094478, -1.020558061026470176, -34.56909192082969895 ) ) ;
#4881 = CARTESIAN_POINT ( 'NONE',  ( 3.750000000000000000, 7.750000000000000000, -3.500000000000000444 ) ) ;
#4882 = CARTESIAN_POINT ( 'NONE',  ( 2.651650429449553314, 5.375000000000000000, -0.8483495705504476847 ) ) ;
#4883 = CC_DESIGN_DATE_AND_TIME_ASSIGNMENT ( #11766, #1039, ( #8149 ) ) ;
#4884 = DIRECTION ( 'NONE',  ( 0.000000000000000000, 1.000000000000000000, 0.000000000000000000 ) ) ;
#4885 = ORIENTED_EDGE ( 'NONE', *, *, #7532, .F. ) ;
#4886 = CARTESIAN_POINT ( 'NONE',  ( -4.234402844927158682, 4.336808689942017736E-16, -117.4888040839639558 ) ) ;
#4887 = CARTESIAN_POINT ( 'NONE',  ( -3.249999999999999112, 2.687500000000000888, -2.153805922287440833 ) ) ;
#4888 = EDGE_CURVE ( 'NONE', #13160, #1079, #597, .T. ) ;
#4889 = CARTESIAN_POINT ( 'NONE',  ( -64.56669032373720540, 14.99999999999999822, -198.1238327362431448 ) ) ;
#4890 = EDGE_CURVE ( 'NONE', #12332, #11957, #8647, .T. ) ;
#4891 = EDGE_CURVE ( 'NONE', #13423, #688, #773, .T. ) ;
#4892 = CARTESIAN_POINT ( 'NONE',  ( 8.432993291281569270, 8.673617379884034486E-16, -127.3575301229172538 ) ) ;
#4893 = CARTESIAN_POINT ( 'NONE',  ( 2.298097038856279362, 9.875000000000000000, -1.201902961143720860 ) ) ;
#4894 = CARTESIAN_POINT ( 'NONE',  ( -4.658423462441079188, 15.00000000000000355, -116.0378842123784153 ) ) ;
#4895 = CARTESIAN_POINT ( 'NONE',  ( -4.665009674110688564, 6.318137159033122024E-12, -129.3402154207890362 ) ) ;
#4896 = CARTESIAN_POINT ( 'NONE',  ( 18.82489474304439270, 0.000000000000000000, -131.0518286717526735 ) ) ;
#4897 = VERTEX_POINT ( 'NONE', #4798 ) ;
#4898 = CARTESIAN_POINT ( 'NONE',  ( -1.526322420895694476, 14.99999999999999822, -106.9293630793504803 ) ) ;
#4899 = LINE ( 'NONE', #2665, #11864 ) ;
#4900 = ORIENTED_EDGE ( 'NONE', *, *, #8545, .T. ) ;
#4901 = ORIENTED_EDGE ( 'NONE', *, *, #13875, .F. ) ;
#4902 = CARTESIAN_POINT ( 'NONE',  ( 25.92962511641389156, 2.144787619503913501, -138.3608807550390907 ) ) ;
#4903 = CARTESIAN_POINT ( 'NONE',  ( 1.553300858899109516, 7.437500000000000000, 0.2499999999999993616 ) ) ;
#4904 = CARTESIAN_POINT ( 'NONE',  ( 2.298097038856278029, 9.125000000000000000, -5.798097038856279362 ) ) ;
#4905 = ORIENTED_EDGE ( 'NONE', *, *, #13276, .F. ) ;
#4906 = CARTESIAN_POINT ( 'NONE',  ( 6.182874915598739918, 13.31144022244639658, 4.038793072555847630 ) ) ;
#4907 = CARTESIAN_POINT ( 'NONE',  ( 3.249999999999998668, 7.687500000000000000, -4.846194077712560500 ) ) ;
#4908 = CARTESIAN_POINT ( 'NONE',  ( -11.55175835850915789, 2.500000000000000444, -126.4710449362810607 ) ) ;
#4909 = CARTESIAN_POINT ( 'NONE',  ( 9.540264233613143574, 0.02433988461803952494, -163.5377607276927563 ) ) ;
#4910 = CARTESIAN_POINT ( 'NONE',  ( -53.96941264214194689, 14.99999999999999645, -161.9875822135848296 ) ) ;
#4911 = VECTOR ( 'NONE', #13152, 1000.000000000000000 ) ;
#4912 = CALENDAR_DATE ( 2026, 8, 10 ) ;
#4913 = CC_DESIGN_PERSON_AND_ORGANIZATION_ASSIGNMENT ( #4924, #1611, ( #1046 ) ) ;
#4914 = CARTESIAN_POINT ( 'NONE',  ( -45.51406255979139814, 15.00000000000000355, -146.4767954873762790 ) ) ;
#4915 = VERTEX_POINT ( 'NONE', #3563 ) ;
#4916 = CARTESIAN_POINT ( 'NONE',  ( 3.249999999999998668, 9.687500000000000000, -4.846194077712560500 ) ) ;
#4917 = CARTESIAN_POINT ( 'NONE',  ( -1.346194077712559389, 1.062500000000000222, -0.2500000000000002220 ) ) ;
#4918 = CARTESIAN_POINT ( 'NONE',  ( -3.323869592214536706, 15.00000000000000533, -120.2528461472343082 ) ) ;
#4919 = CARTESIAN_POINT ( 'NONE',  ( -2.651650429449552870, 13.87500000000000178, -6.151650429449552426 ) ) ;
#4920 = CARTESIAN_POINT ( 'NONE',  ( -63.21422130130007133, 9.999999999999998224, -203.6040552426024988 ) ) ;
#4921 = FACE_OUTER_BOUND ( 'NONE', #2447, .T. ) ;
#4922 = CARTESIAN_POINT ( 'NONE',  ( 3.249999999999998224, 1.312500000000000444, -2.153805922287439945 ) ) ;
#4923 = CARTESIAN_POINT ( 'NONE',  ( 10.20171492915204503, 1.831415644534537757, -106.3803253616011943 ) ) ;
#4924 = PERSON_AND_ORGANIZATION ( #3176, #3020 ) ;
#4925 = CC_DESIGN_APPROVAL ( #668, ( #11099 ) ) ;
#4926 = CARTESIAN_POINT ( 'NONE',  ( -1.779087990637969519, 14.96619511928228263, -125.4805735508361693 ) ) ;
#4927 = CARTESIAN_POINT ( 'NONE',  ( -1.500000000000000000, 4.500000000000000888, 0.2500000000000002220 ) ) ;
#4928 = AXIS2_PLACEMENT_3D ( 'NONE', #1902, #8067, #4302 ) ;
#4929 = ORIENTED_EDGE ( 'NONE', *, *, #2502, .T. ) ;
#4930 = CARTESIAN_POINT ( 'NONE',  ( 5.394780522009475554, 1.937363519424163405, 4.074339615067635201 ) ) ;
#4931 = CARTESIAN_POINT ( 'NONE',  ( -3.249999999999999556, 6.250000000000000000, -3.499999999999999556 ) ) ;
#4932 = EDGE_CURVE ( 'NONE', #5961, #6131, #1244, .T. ) ;
#4933 = CARTESIAN_POINT ( 'NONE',  ( -69.71822546521497088, 9.999999999999996447, -185.9780503014303861 ) ) ;
#4934 = CARTESIAN_POINT ( 'NONE',  ( 2.298097038856278029, 1.124999999999999778, -5.798097038856279362 ) ) ;
#4935 = CARTESIAN_POINT ( 'NONE',  ( -1.346194077712558945, 7.562500000000000888, -0.2500000000000002220 ) ) ;
#4936 = CARTESIAN_POINT ( 'NONE',  ( -5.611193301530131627, 15.00000000000000000, -110.1737759618165171 ) ) ;
#4937 = CARTESIAN_POINT ( 'NONE',  ( 3.902492714259738538, 14.90432320739552452, -1.582372767571640138 ) ) ;
#4938 = SECURITY_CLASSIFICATION ( '', '', #9304 ) ;
#4939 = CARTESIAN_POINT ( 'NONE',  ( -16.94138229547579400, 15.00000000000000000, -154.2864167784019287 ) ) ;
#4940 = CARTESIAN_POINT ( 'NONE',  ( 1.346194077712560944, 1.937500000000000000, -0.2500000000000010547 ) ) ;
#4941 = CARTESIAN_POINT ( 'NONE',  ( -3.750000000000000000, 1.687499999999999778, -1.946699141100893149 ) ) ;
#4942 = CIRCLE ( 'NONE', #6918, 0.5000000000000012212 ) ;
#4943 = CARTESIAN_POINT ( 'NONE',  ( 1.553300858899105963, 6.562500000000000000, -7.250000000000000000 ) ) ;
#4944 = CARTESIAN_POINT ( 'NONE',  ( -3.880844424049542329, 11.25546320798563649, -45.77986880073594733 ) ) ;
#4945 = CARTESIAN_POINT ( 'NONE',  ( -1.553300858899107073, 4.937500000000000888, -7.249999999999999112 ) ) ;
#4946 = CARTESIAN_POINT ( 'NONE',  ( 2.958685104891044748, 14.61614439227996520, 2.621129781322379948 ) ) ;
#4947 = CARTESIAN_POINT ( 'NONE',  ( 9.068716941525982733, 1.734723475976807094E-15, -163.1923081219560174 ) ) ;
#4948 = CARTESIAN_POINT ( 'NONE',  ( 4.507463604512255806, 5.000000000000000000, 2.585105772303601945 ) ) ;
#4949 = VECTOR ( 'NONE', #1025, 1000.000000000000000 ) ;
#4950 = CARTESIAN_POINT ( 'NONE',  ( 1.243260443319662123, 4.000000000000000000, -139.4020581015306846 ) ) ;
#4951 = VECTOR ( 'NONE', #10044, 1000.000000000000000 ) ;
#4952 = CARTESIAN_POINT ( 'NONE',  ( 8.735174570882092482, 3.542760715477264011, 2.737195459111058771 ) ) ;
#4953 = CARTESIAN_POINT ( 'NONE',  ( 8.595858757338769252, -1.010734139224366919E-11, -113.5677547687552646 ) ) ;
#4954 = ORIENTED_EDGE ( 'NONE', *, *, #3564, .T. ) ;
#4955 = B_SPLINE_CURVE_WITH_KNOTS ( 'NONE', 3,
 ( #1357, #6061, #15286, #196, #4678, #3601, #10483, #1198, #4906, #4609, #7130, #5900, #14041, #10623, #5982, #11934, #2519, #3671 ),
 .UNSPECIFIED., .F., .F.,
 ( 4, 2, 2, 2, 2, 2, 2, 2, 4 ),
 ( 0.000000000000000000, 0.0009867360918462263642, 0.001973472183692452728, 0.002960208275538679309, 0.003946944367384905457, 0.004933680459231131604, 0.005920416551077358619, 0.006907152642923583899, 0.007893888734769809179 ),
 .UNSPECIFIED. ) ;
#4956 = EDGE_CURVE ( 'NONE', #6908, #11832, #7420, .T. ) ;
#4957 = CARTESIAN_POINT ( 'NONE',  ( -2.651650429449553314, 10.87499999999999822, -6.151650429449552426 ) ) ;
#4958 = ORIENTED_EDGE ( 'NONE', *, *, #5908, .F. ) ;
#4959 = CARTESIAN_POINT ( 'NONE',  ( -5.336847314811834053, 2.500000000000000444, -115.5414184962005635 ) ) ;
#4960 = CARTESIAN_POINT ( 'NONE',  ( -17.29863105483956787, -2.690463824762831016E-12, -194.2807859071518521 ) ) ;
#4961 = CARTESIAN_POINT ( 'NONE',  ( -2.651650429449553314, 10.37500000000000000, -6.151650429449552426 ) ) ;
#4962 = CARTESIAN_POINT ( 'NONE',  ( 2.651650429449553314, 6.374999999999999112, -0.8483495705504476847 ) ) ;
#4963 = CARTESIAN_POINT ( 'NONE',  ( -17.32624372124044854, 0.6199615622964459449, -130.2318118670719116 ) ) ;
#4964 = ORIENTED_EDGE ( 'NONE', *, *, #317, .T. ) ;
#4965 = CARTESIAN_POINT ( 'NONE',  ( -6.465967782647407347, 0.3928012870235511600, -116.8537262797278800 ) ) ;
#4966 = CARTESIAN_POINT ( 'NONE',  ( 1.346194077712561166, 3.437500000000000444, -0.2500000000000011102 ) ) ;
#4967 = CIRCLE ( 'NONE', #38, 14.80000000000025651 ) ;
#4968 = CARTESIAN_POINT ( 'NONE',  ( 0.000000000000000000, 11.00000000000000000, 0.2500000000000002220 ) ) ;
#4969 = CARTESIAN_POINT ( 'NONE',  ( -69.46795959346728466, 9.999999999999998224, -199.1268727649999732 ) ) ;
#4970 = CARTESIAN_POINT ( 'NONE',  ( 3.810793737614490695, 8.673617379884037444E-16, -110.0325487313770481 ) ) ;
#4971 = CARTESIAN_POINT ( 'NONE',  ( -2.298097038856278473, 9.125000000000000000, -1.201902961143720416 ) ) ;
#4972 = FACE_OUTER_BOUND ( 'NONE', #2672, .T. ) ;
#4973 = CARTESIAN_POINT ( 'NONE',  ( -6.451063615524601502, 4.999999999999201528, -125.7472547710055721 ) ) ;
#4974 = CARTESIAN_POINT ( 'NONE',  ( 10.46664703702157695, -1.287459477862190473E-12, -121.2724779345652024 ) ) ;
#4975 = ORIENTED_EDGE ( 'NONE', *, *, #3286, .T. ) ;
#4976 = CARTESIAN_POINT ( 'NONE',  ( 1.243260443319662123, 4.179859613694246079, -139.4020581015306846 ) ) ;
#4977 = CARTESIAN_POINT ( 'NONE',  ( -25.82983890416511841, 9.999999999999998224, -142.4527639562402328 ) ) ;
#4978 = CIRCLE ( 'NONE', #7449, 3.750000000000003109 ) ;
#4979 = EDGE_LOOP ( 'NONE', ( #2588, #9829, #9545 ) ) ;
#4980 = EDGE_CURVE ( 'NONE', #6553, #8666, #14081, .T. ) ;
#4981 = CARTESIAN_POINT ( 'NONE',  ( -25.42939282183900573, 4.000000000000000000, -209.0516719515502473 ) ) ;
#4982 = CARTESIAN_POINT ( 'NONE',  ( 0.1251546907736567626, 0.2964742070510372751, -6.863050255469943295 ) ) ;
#4983 =( BOUNDED_SURFACE ( )  B_SPLINE_SURFACE ( 3, 1, ( 
 ( #12266, #11032 ),
 ( #14606, #8621 ),
 ( #13519, #14683 ),
 ( #4086, #5313 ) ),
 .UNSPECIFIED., .F., .F., .T. ) 
 B_SPLINE_SURFACE_WITH_KNOTS ( ( 4, 4 ),
 ( 2, 2 ),
 ( 0.000000000000000000, 1.000000000000000000 ),
 ( 0.000000000000000000, 1.000000000000000000 ),
 .UNSPECIFIED. ) 
 GEOMETRIC_REPRESENTATION_ITEM ( )  RATIONAL_B_SPLINE_SURFACE ( (
 ( 1.000000000000000000, 1.000000000000000000),
 ( 0.9216682375510407699, 0.9216682375510407699),
 ( 0.9216682375510407699, 0.9216682375510407699),
 ( 1.000000000000000000, 1.000000000000000000) ) ) 
 REPRESENTATION_ITEM ( '' )  SURFACE ( )  );
#4984 = CARTESIAN_POINT ( 'NONE',  ( 1.553300858899109071, 14.43750000000000178, 0.2499999999999989175 ) ) ;
#4985 = CARTESIAN_POINT ( 'NONE',  ( -2.298097038856279362, 7.874999999999999112, -5.798097038856278473 ) ) ;
#4986 = ADVANCED_FACE ( 'NONE', ( #9581, #3485 ), #7031, .T. ) ;
#4987 = CARTESIAN_POINT ( 'NONE',  ( 3.249999999999998224, 11.18750000000000178, -4.846194077712561388 ) ) ;
#4989 = EDGE_CURVE ( 'NONE', #6272, #10654, #9641, .T. ) ;
#4988 = ORIENTED_EDGE ( 'NONE', *, *, #7044, .F. ) ;
#4990 = CARTESIAN_POINT ( 'NONE',  ( -10.68385489208660211, 8.673617379884034486E-16, -179.9329437176981799 ) ) ;
#4991 = CARTESIAN_POINT ( 'NONE',  ( -2.298097038856278918, 5.375000000000000000, -5.798097038856277585 ) ) ;
#4992 = PRODUCT ( 'Nut_Predeterminado', 'Nut_Predeterminado', '', ( #3143 ) ) ;
#4993 = CC_DESIGN_DATE_AND_TIME_ASSIGNMENT ( #7014, #5925, ( #7950 ) ) ;
#4994 = CARTESIAN_POINT ( 'NONE',  ( -9.240119717576689595, 2.500000000000000444, -104.6630069175297564 ) ) ;
#4995 = CARTESIAN_POINT ( 'NONE',  ( -50.73799765964188424, 10.00000000000000000, -166.0021564914866872 ) ) ;
#4996 = CARTESIAN_POINT ( 'NONE',  ( -55.81483411153980256, 14.99999999999999822, -164.4788693041486454 ) ) ;
#4997 = PERSON_AND_ORGANIZATION ( #3176, #3020 ) ;
#4998 = CARTESIAN_POINT ( 'NONE',  ( 0.000000000000000000, 0.000000000000000000, 0.000000000000000000 ) ) ;
#4999 = ORIENTED_EDGE ( 'NONE', *, *, #5285, .T. ) ;
#5000 = CARTESIAN_POINT ( 'NONE',  ( 3.249999999999998224, 13.18750000000000000, -4.846194077712561388 ) ) ;
#5001 = CARTESIAN_POINT ( 'NONE',  ( -3.749999999999999556, 12.18750000000000000, -1.946699141100892927 ) ) ;
#5002 = ADVANCED_FACE ( 'NONE', ( #7097 ), #7225, .T. ) ;
#5003 = PRODUCT_DEFINITION_FORMATION_WITH_SPECIFIED_SOURCE ( 'ANY', '', #8425, .NOT_KNOWN. ) ;
#5004 = CARTESIAN_POINT ( 'NONE',  ( -25.82983890416511841, 5.000000000000000000, -157.2527639562405000 ) ) ;
#5005 = CARTESIAN_POINT ( 'NONE',  ( 3.749999999999999556, 13.25000000000000178, -3.500000000000000444 ) ) ;
#5006 = TOROIDAL_SURFACE ( 'NONE', #569, 2.000000000000016431, 5.000000000000000000 ) ;
#5007 = CARTESIAN_POINT ( 'NONE',  ( -65.24151687956603496, 15.39242333475949565, -205.1717068079038597 ) ) ;
#5008 = PLANE ( 'NONE',  #1757 ) ;
#5009 = CARTESIAN_POINT ( 'NONE',  ( -3.249999999999999112, 3.687500000000000444, -2.153805922287440833 ) ) ;
#5010 = CARTESIAN_POINT ( 'NONE',  ( 7.837953251846155212, 0.2318755756027173209, -105.5268984575482420 ) ) ;
#5011 = APPLICATION_PROTOCOL_DEFINITION ( 'international standard', 'config_control_design', 1994, #1665 ) ;
#5012 = CARTESIAN_POINT ( 'NONE',  ( -63.60348060676458459, 15.00000000000000000, -180.2685449772604045 ) ) ;
#5013 = DIRECTION ( 'NONE',  ( 0.000000000000000000, 0.000000000000000000, 1.000000000000000000 ) ) ;
#5014 = ORIENTED_EDGE ( 'NONE', *, *, #1065, .T. ) ;
#5015 = CARTESIAN_POINT ( 'NONE',  ( 4.911596535478627068, 1.131903148223331934, 3.093215885358307382 ) ) ;
#5016 = CARTESIAN_POINT ( 'NONE',  ( -3.980102097228897245E-16, 7.500000000000000000, -6.749999999999999112 ) ) ;
#5017 = TOROIDAL_SURFACE ( 'NONE', #334, 5.999999999999995559, 5.000000000000000000 ) ;
#5018 = CARTESIAN_POINT ( 'NONE',  ( -7.997017844161499411, 0.4580377704404314243, -104.9354529933016380 ) ) ;
#5019 = CARTESIAN_POINT ( 'NONE',  ( 1.346194077712558279, 1.062500000000000444, -6.750000000000000888 ) ) ;
#5020 = CARTESIAN_POINT ( 'NONE',  ( -3.249999999999999112, 9.687500000000000000, -2.153805922287440833 ) ) ;
#5021 = CARTESIAN_POINT ( 'NONE',  ( -7.230047174306548641, 15.00000000000000000, -120.6008656443442959 ) ) ;
#5022 = CARTESIAN_POINT ( 'NONE',  ( 1.419014798623991824, 13.29791182762822288, 2.129561375652841981 ) ) ;
#5023 = CARTESIAN_POINT ( 'NONE',  ( -4.827681327713614579, 15.00000000000000000, -144.0483944136883565 ) ) ;
#5024 = CARTESIAN_POINT ( 'NONE',  ( 3.249999999999998668, 4.687500000000000888, -4.846194077712560500 ) ) ;
#5025 = CARTESIAN_POINT ( 'NONE',  ( -4.592425496802573972E-16, 2.000000000000000000, -7.250000000000000000 ) ) ;
#5026 = CARTESIAN_POINT ( 'NONE',  ( -3.750000000000000000, 5.187500000000000888, -1.946699141100892927 ) ) ;
#5027 = CARTESIAN_POINT ( 'NONE',  ( -3.421776217561549149, 10.60802507245954374, -46.00634398649022927 ) ) ;
#5028 = CARTESIAN_POINT ( 'NONE',  ( -2.651650429449552870, 7.625000000000001776, -0.8483495705504463524 ) ) ;
#5029 = AXIS2_PLACEMENT_3D ( 'NONE', #1622, #6335, #10039 ) ;
#5030 = CARTESIAN_POINT ( 'NONE',  ( 0.6250914642584898262, 11.93308722886469120, 2.723738529685005183 ) ) ;
#5031 = AXIS2_PLACEMENT_3D ( 'NONE', #1094, #1237, #10519 ) ;
#5032 = CARTESIAN_POINT ( 'NONE',  ( 13.02262923224196811, 4.033366868162254981, -166.4500998287084883 ) ) ;
#5033 = CARTESIAN_POINT ( 'NONE',  ( 9.044950117654433797, -4.000000000000000000, -144.9826476090360643 ) ) ;
#5034 = DIRECTION ( 'NONE',  ( -0.000000000000000000, -1.000000000000000000, -0.000000000000000000 ) ) ;
#5035 = CARTESIAN_POINT ( 'NONE',  ( 11.44399236068192671, -4.000000000000000000, -138.9341978221715976 ) ) ;
#5036 = CARTESIAN_POINT ( 'NONE',  ( -25.46076704144856961, 8.673617379884034486E-16, -188.0253354884488601 ) ) ;
#5037 = CARTESIAN_POINT ( 'NONE',  ( -1.376260179405575323, 8.673617379884035472E-16, -106.6458321843530541 ) ) ;
#5038 = VERTEX_POINT ( 'NONE', #13308 ) ;
#5039 = CARTESIAN_POINT ( 'NONE',  ( 3.750000000000000000, 10.31250000000000000, -1.946699141100892705 ) ) ;
#5040 = VERTEX_POINT ( 'NONE', #398 ) ;
#5041 = CARTESIAN_POINT ( 'NONE',  ( -6.947321920292441888, 2.500000000000000444, -120.0269581758342525 ) ) ;
#5042 = CARTESIAN_POINT ( 'NONE',  ( -0.9087754948914893438, -1.020558061026470176, -45.55632290616385660 ) ) ;
#5043 = CARTESIAN_POINT ( 'NONE',  ( -2.651650429449553314, 8.375000000000000000, -6.151650429449552426 ) ) ;
#5044 = AXIS2_PLACEMENT_3D ( 'NONE', #10178, #8007, #10323 ) ;
#5045 = CARTESIAN_POINT ( 'NONE',  ( -3.749999999999999556, 9.750000000000000000, -3.499999999999999112 ) ) ;
#5046 = CARTESIAN_POINT ( 'NONE',  ( 17.50071171097425804, 8.749999999999998224, -91.70093451412481045 ) ) ;
#5047 = EDGE_LOOP ( 'NONE', ( #2569, #8456, #678, #3921 ) ) ;
#5048 = CARTESIAN_POINT ( 'NONE',  ( -8.208951728224439748, 1.532620112797828726, -116.7121244410437129 ) ) ;
#5049 = CARTESIAN_POINT ( 'NONE',  ( 2.298097038856279362, 5.375000000000000000, -1.201902961143720860 ) ) ;
#5050 = CARTESIAN_POINT ( 'NONE',  ( -3.749999999999999556, 8.187500000000000000, -1.946699141100892927 ) ) ;
#5051 = CARTESIAN_POINT ( 'NONE',  ( -69.84691631900385289, 9.999999999999998224, -196.7709020262129229 ) ) ;
#5052 = DIRECTION ( 'NONE',  ( -0.3090169943749621062, 0.000000000000000000, -0.9510565162951489793 ) ) ;
#5053 = EDGE_CURVE ( 'NONE', #922, #9221, #2757, .T. ) ;
#5054 = DIRECTION ( 'NONE',  ( 0.9999946794944214457, 0.000000000000000000, 0.003262051938530596308 ) ) ;
#5055 = CARTESIAN_POINT ( 'NONE',  ( 3.249999999999999556, 7.750000000000000000, -3.500000000000000000 ) ) ;
#5056 = AXIS2_PLACEMENT_3D ( 'NONE', #804, #11456, #13561 ) ;
#5057 = APPROVAL_STATUS ( 'not_yet_approved' ) ;
#5058 = CARTESIAN_POINT ( 'NONE',  ( 4.312410837866842428, -4.336808689942017736E-15, -133.7542242696550829 ) ) ;
#5059 = CARTESIAN_POINT ( 'NONE',  ( 10.01939027896081313, 15.00000000000000000, -127.6977514918621637 ) ) ;
#5060 = VERTEX_POINT ( 'NONE', #5107 ) ;
#5061 = LINE ( 'NONE', #7447, #14599 ) ;
#5062 = DIRECTION ( 'NONE',  ( 0.000000000000000000, 0.000000000000000000, 1.000000000000000000 ) ) ;
#5063 = EDGE_LOOP ( 'NONE', ( #8821, #10774, #4954, #10200, #9082 ) ) ;
#5064 = ORIENTED_EDGE ( 'NONE', *, *, #9243, .F. ) ;
#5065 = CARTESIAN_POINT ( 'NONE',  ( 8.895558325401111688, 6.000000000000000000, -141.4560052469132643 ) ) ;
#5066 = CARTESIAN_POINT ( 'NONE',  ( -2.651650429449552870, 11.62500000000000000, -0.8483495705504467965 ) ) ;
#5067 = CARTESIAN_POINT ( 'NONE',  ( 1.346194077712558279, 13.06250000000000178, -6.750000000000000888 ) ) ;
#5068 = CARTESIAN_POINT ( 'NONE',  ( -3.980102097228897738E-16, 12.00000000000000178, -6.749999999999999112 ) ) ;
#5069 = EDGE_LOOP ( 'NONE', ( #4546, #2666 ) ) ;
#5070 = DIRECTION ( 'NONE',  ( -0.000000000000000000, 1.000000000000000000, -0.000000000000000000 ) ) ;
#5071 = CARTESIAN_POINT ( 'NONE',  ( 3.249999999999999556, 5.750000000000000000, -3.500000000000000000 ) ) ;
#5072 = CARTESIAN_POINT ( 'NONE',  ( -5.946715039918482937, 2.500000000000000000, -117.8159155480562958 ) ) ;
#5073 = EDGE_CURVE ( 'NONE', #6929, #1356, #1515, .T. ) ;
#5074 = CARTESIAN_POINT ( 'NONE',  ( 9.068716941525991615, 0.000000000000000000, -163.1923081219560174 ) ) ;
#5075 = CARTESIAN_POINT ( 'NONE',  ( -0.3766621274091715987, 0.5000000000000000000, 0.1491815183709511716 ) ) ;
#5076 = APPROVAL_STATUS ( 'not_yet_approved' ) ;
#5077 = CARTESIAN_POINT ( 'NONE',  ( -24.63184704799750691, 3.774669349862838974, -208.8347861833674131 ) ) ;
#5078 =( BOUNDED_SURFACE ( )  B_SPLINE_SURFACE ( 3, 2, ( 
 ( #13513, #3759, #8466 ),
 ( #13198, #1828, #671 ),
 ( #9005, #14755, #7771 ),
 ( #9156, #11250, #14903 ),
 ( #4301, #6688, #7844 ),
 ( #8930, #4372, #13658 ),
 ( #10020, #13581, #13884 ),
 ( #4153, #15048, #4443 ),
 ( #5526, #11402, #8853 ),
 ( #1973, #821, #10245 ),
 ( #13731, #10091, #9080 ),
 ( #4225, #2050, #3059 ),
 ( #14977, #6615, #2127 ),
 ( #3130, #12715, #10171 ),
 ( #3279, #13801, #742 ),
 ( #1901, #12484, #7994 ),
 ( #3201, #6538, #12560 ),
 ( #7918, #2983, #6830 ),
 ( #12638, #11322, #7692 ),
 ( #10310, #12405, #11546 ),
 ( #5449, #5377, #14825 ),
 ( #6764, #11476, #961 ),
 ( #895, #5595, #13959 ),
 ( #5970, #9459, #4823 ),
 ( #1041, #6903, #109 ),
 ( #13091, #12866, #4745 ),
 ( #12789, #3660, #15204 ),
 ( #2278, #6983, #5819 ) ),
 .UNSPECIFIED., .F., .F., .T. ) 
 B_SPLINE_SURFACE_WITH_KNOTS ( ( 4, 2, 2, 2, 2, 2, 2, 2, 2, 2, 2, 2, 2, 4 ),
 ( 3, 3 ),
 ( 0.05714059389823637758, 0.06030189704985427362, 0.06188254862566322512, 0.06346320020147216967, 0.06662450335309007265, 0.06978580650470797564, 0.07136645808051692019, 0.07294710965632586475, 0.07452776123213480930, 0.07610841280794376773, 0.07926971595956167072, 0.08006004174746614299, 0.08085036753537061527, 0.08243101911117955982 ),
 ( 0.000000000000000000, 1.000000000000000000 ),
 .UNSPECIFIED. ) 
 GEOMETRIC_REPRESENTATION_ITEM ( )  RATIONAL_B_SPLINE_SURFACE ( (
 ( 1.000000000000000000, 0.7071067811865475727, 1.000000000000000000),
 ( 1.000000000000000000, 0.7071067811865475727, 1.000000000000000000),
 ( 1.000000000000000000, 0.7071067811865475727, 1.000000000000000000),
 ( 1.000000000000000000, 0.7071067811865475727, 1.000000000000000000),
 ( 1.000000000000000000, 0.7071067811865464625, 1.000000000000000000),
 ( 1.000000000000000000, 0.7071067811865464625, 1.000000000000000000),
 ( 1.000000000000000000, 0.7071067811865475727, 1.000000000000000000),
 ( 1.000000000000000000, 0.7071067811865475727, 1.000000000000000000),
 ( 1.000000000000000000, 0.7071067811865473507, 1.000000000000000000),
 ( 1.000000000000000000, 0.7071067811865473507, 1.000000000000000000),
 ( 1.000000000000000000, 0.7071067811865471286, 1.000000000000000000),
 ( 1.000000000000000000, 0.7071067811865471286, 1.000000000000000000),
 ( 1.000000000000000000, 0.7071067811865473507, 1.000000000000000000),
 ( 1.000000000000000000, 0.7071067811865473507, 1.000000000000000000),
 ( 1.000000000000000000, 0.7071067811865475727, 1.000000000000000000),
 ( 1.000000000000000000, 0.7071067811865475727, 1.000000000000000000),
 ( 1.000000000000000000, 0.7071067811865476838, 1.000000000000000000),
 ( 1.000000000000000000, 0.7071067811865476838, 1.000000000000000000),
 ( 1.000000000000000000, 0.7071067811865475727, 1.000000000000000000),
 ( 1.000000000000000000, 0.7071067811865475727, 1.000000000000000000),
 ( 1.000000000000000000, 0.7071067811865475727, 1.000000000000000000),
 ( 1.000000000000000000, 0.7071067811865475727, 1.000000000000000000),
 ( 1.000000000000000000, 0.7071067811865475727, 1.000000000000000000),
 ( 1.000000000000000000, 0.7071067811865475727, 1.000000000000000000),
 ( 1.000000000000000000, 0.7071067811865487940, 1.000000000000000000),
 ( 1.000000000000000000, 0.7071067811865487940, 1.000000000000000000),
 ( 1.000000000000000000, 0.7071067811865475727, 1.000000000000000000),
 ( 1.000000000000000000, 0.7071067811865475727, 1.000000000000000000) ) ) 
 REPRESENTATION_ITEM ( '' )  SURFACE ( )  );
#5079 = ORIENTED_EDGE ( 'NONE', *, *, #5448, .T. ) ;
#5080 = CARTESIAN_POINT ( 'NONE',  ( -2.298097038856278918, 9.375000000000000000, -5.798097038856277585 ) ) ;
#5081 = CARTESIAN_POINT ( 'NONE',  ( 3.249999999999998668, 1.687500000000000000, -4.846194077712560500 ) ) ;
#5082 = CARTESIAN_POINT ( 'NONE',  ( 2.651650429449552870, 11.62500000000000000, -6.151650429449554203 ) ) ;
#5083 = CARTESIAN_POINT ( 'NONE',  ( -1.302272502657875197, 1.750000000000000000, -1.200882754745186798 ) ) ;
#5084 = CARTESIAN_POINT ( 'NONE',  ( 3.749999999999998668, 3.687500000000000444, -5.053300858899107517 ) ) ;
#5085 = CARTESIAN_POINT ( 'NONE',  ( -67.63088312920152134, 12.20966866773095560, -203.2556435494578579 ) ) ;
#5086 = CARTESIAN_POINT ( 'NONE',  ( -35.49029739244800652, 9.999999999999998224, -131.2404697308744517 ) ) ;
#5087 = CARTESIAN_POINT ( 'NONE',  ( 8.469560671982707234, 0.4830037559895700716, -105.5866725495891245 ) ) ;
#5088 = ADVANCED_FACE ( 'NONE', ( #6491 ), #14153, .F. ) ;
#5089 = COORDINATED_UNIVERSAL_TIME_OFFSET ( 0, 0, .AHEAD. ) ;
#5090 = LINE ( 'NONE', #10031, #12684 ) ;
#5091 = CARTESIAN_POINT ( 'NONE',  ( -0.3766621274091715987, -0.2500000000000000000, 0.1491815183709511716 ) ) ;
#5092 = ORIENTED_EDGE ( 'NONE', *, *, #13294, .T. ) ;
#5093 = CARTESIAN_POINT ( 'NONE',  ( 4.516489297218283738, -0.0008961263519764209014, -1.658221315986036393 ) ) ;
#5094 = CARTESIAN_POINT ( 'NONE',  ( -3.249999999999999556, 5.250000000000000000, -3.499999999999999556 ) ) ;
#5095 = CARTESIAN_POINT ( 'NONE',  ( -8.671996357861377902, 0.9205354582397626828, -104.5402285118089623 ) ) ;
#5096 = CARTESIAN_POINT ( 'NONE',  ( 3.249999999999999112, 14.81250000000000000, -2.153805922287439945 ) ) ;
#5097 = CARTESIAN_POINT ( 'NONE',  ( 1.346194077712558279, 9.062500000000000000, -6.750000000000000888 ) ) ;
#5098 = DIRECTION ( 'NONE',  ( 0.000000000000000000, -1.000000000000000000, 0.000000000000000000 ) ) ;
#5099 = DIRECTION ( 'NONE',  ( 0.02693067314567074849, -0.8090169943749466741, -0.5871679841888934881 ) ) ;
#5100 = CARTESIAN_POINT ( 'NONE',  ( 10.73687333765669294, 14.11987504264111060, -106.5879302472600756 ) ) ;
#5101 = CARTESIAN_POINT ( 'NONE',  ( -3.249999999999999556, 5.250000000000000000, -3.499999999999999556 ) ) ;
#5102 = CARTESIAN_POINT ( 'NONE',  ( 2.651650429449552870, 3.125000000000000444, -6.151650429449553314 ) ) ;
#5103 = CARTESIAN_POINT ( 'NONE',  ( -1.553300858899107073, 4.437500000000001776, -7.250000000000000000 ) ) ;
#5104 = CARTESIAN_POINT ( 'NONE',  ( -3.589008443032619233, 10.29141329574603958, -47.02125063507394032 ) ) ;
#5105 = CARTESIAN_POINT ( 'NONE',  ( 0.000000000000000000, 5.500000000000000888, 0.2500000000000002220 ) ) ;
#5106 = CARTESIAN_POINT ( 'NONE',  ( 4.127667803487161002, 14.97371045984202098, 0.2463234276174943727 ) ) ;
#5107 = CARTESIAN_POINT ( 'NONE',  ( -18.09353981420494151, 2.500000000000000444, -129.3374956033359240 ) ) ;
#5108 = CARTESIAN_POINT ( 'NONE',  ( 14.22910372453204353, 6.000000000000000000, -126.5134921567817941 ) ) ;
#5109 = CARTESIAN_POINT ( 'NONE',  ( -6.790153584124027475, 6.000000000000000000, -124.9643354754709748 ) ) ;
#5110 = CARTESIAN_POINT ( 'NONE',  ( 26.58801926426209405, 5.000000000000000888, -139.0072983920785532 ) ) ;
#5111 = CARTESIAN_POINT ( 'NONE',  ( 51.10947674412996378, 1.750000000000000000, 71.89891518833638884 ) ) ;
#5112 = ORIENTED_EDGE ( 'NONE', *, *, #2197, .T. ) ;
#5113 = CARTESIAN_POINT ( 'NONE',  ( 2.298097038856279362, 0.3750000000000001110, -1.201902961143720860 ) ) ;
#5114 = EDGE_LOOP ( 'NONE', ( #2202, #5601, #11760, #8177 ) ) ;
#5115 = DIRECTION ( 'NONE',  ( 0.9961255586397055328, -0.000000000000000000, -0.08794243244722428632 ) ) ;
#5116 = CARTESIAN_POINT ( 'NONE',  ( -25.49759732579816074, -1.965429835991842803E-15, -208.9099396872309740 ) ) ;
#5117 = CARTESIAN_POINT ( 'NONE',  ( 0.000000000000000000, 8.000000000000000000, 0.2500000000000002220 ) ) ;
#5118 = CARTESIAN_POINT ( 'NONE',  ( -3.749999999999999556, 8.750000000000001776, -3.499999999999999112 ) ) ;
#5119 = CARTESIAN_POINT ( 'NONE',  ( 1.500000000000000000, 4.500000000000000888, 0.2500000000000002220 ) ) ;
#5120 = VERTEX_POINT ( 'NONE', #3525 ) ;
#5121 = CARTESIAN_POINT ( 'NONE',  ( 1.346194077712561166, 5.437500000000000888, -0.2500000000000011102 ) ) ;
#5122 = CARTESIAN_POINT ( 'NONE',  ( 1.553300858899108849, 7.937500000000000888, 0.2499999999999993616 ) ) ;
#5123 = CARTESIAN_POINT ( 'NONE',  ( -70.08092325134745693, 9.999999999999998224, -193.7014402726132971 ) ) ;
#5124 = B_SPLINE_CURVE_WITH_KNOTS ( 'NONE', 3,
 ( #6091, #14469, #10807, #13222 ),
 .UNSPECIFIED., .F., .F.,
 ( 4, 4 ),
 ( 0.000000000000000000, 0.0003766969609235024303 ),
 .UNSPECIFIED. ) ;
#5126 = ADVANCED_FACE ( 'NONE', ( #9326, #2370 ), #12592, .T. ) ;
#5125 = CARTESIAN_POINT ( 'NONE',  ( 9.943023108890811201, 5.000000000000000888, -43.30782091980646697 ) ) ;
#5127 = CALENDAR_DATE ( 2026, 8, 10 ) ;
#5128 = CARTESIAN_POINT ( 'NONE',  ( 2.298097038856278473, 9.625000000000000000, -5.798097038856279362 ) ) ;
#5129 = CARTESIAN_POINT ( 'NONE',  ( -8.589347325819183254, 14.99999999999673683, -120.3237211900380714 ) ) ;
#5130 = DATE_TIME_ROLE ( 'classification_date' ) ;
#5131 = CARTESIAN_POINT ( 'NONE',  ( -4.681294236308613854, 6.071532165918824830E-15, -115.9486516925368846 ) ) ;
#5132 = CARTESIAN_POINT ( 'NONE',  ( 4.006117301121300045, 8.673617379884035472E-16, -109.3626630931961614 ) ) ;
#5133 = ORIENTED_EDGE ( 'NONE', *, *, #11119, .F. ) ;
#5134 = FACE_OUTER_BOUND ( 'NONE', #3810, .T. ) ;
#5135 = CARTESIAN_POINT ( 'NONE',  ( 17.50071171097425804, 8.749999999999998224, -91.70093451412481045 ) ) ;
#5136 = VERTEX_POINT ( 'NONE', #8157 ) ;
#5137 = EDGE_CURVE ( 'NONE', #7290, #7124, #11716, .T. ) ;
#5138 = CARTESIAN_POINT ( 'NONE',  ( 10.00369055844187649, 12.49999999999999822, -46.08764602067113714 ) ) ;
#5139 = CARTESIAN_POINT ( 'NONE',  ( 9.068716941525991615, 0.000000000000000000, -163.1923081219560174 ) ) ;
#5140 = CARTESIAN_POINT ( 'NONE',  ( 1.553300858899109071, 13.43750000000000355, 0.2499999999999989175 ) ) ;
#5141 = CARTESIAN_POINT ( 'NONE',  ( 0.000000000000000000, 12.50000000000000178, -0.2500000000000002220 ) ) ;
#5142 = CARTESIAN_POINT ( 'NONE',  ( 0.000000000000000000, 10.49999999999999822, -0.2500000000000002220 ) ) ;
#5143 = VERTEX_POINT ( 'NONE', #8888 ) ;
#5144 = FACE_OUTER_BOUND ( 'NONE', #10011, .T. ) ;
#5145 = CARTESIAN_POINT ( 'NONE',  ( -3.249999999999999556, 8.312500000000000000, -4.846194077712557835 ) ) ;
#5146 = DIRECTION ( 'NONE',  ( -0.6282721832679390994, 0.000000000000000000, 0.7779936141972743080 ) ) ;
#5147 = CARTESIAN_POINT ( 'NONE',  ( 10.22352057816269699, 15.00000000000000000, -125.5112093480189657 ) ) ;
#5148 = CARTESIAN_POINT ( 'NONE',  ( -35.18331673012945515, 10.00000000000000355, -156.2104531713141000 ) ) ;
#5149 = CARTESIAN_POINT ( 'NONE',  ( -37.17445053438615332, 15.00000000000000533, -151.4226814532358674 ) ) ;
#5150 = PERSON_AND_ORGANIZATION ( #3176, #3020 ) ;
#5151 = CARTESIAN_POINT ( 'NONE',  ( -25.11906781955738310, 0.000000000000000000, -198.9681998140721078 ) ) ;
#5152 = VERTEX_POINT ( 'NONE', #13619 ) ;
#5153 = CARTESIAN_POINT ( 'NONE',  ( -1.346194077712559389, 9.437500000000000000, -6.749999999999999112 ) ) ;
#5154 = CARTESIAN_POINT ( 'NONE',  ( 2.298097038856279362, 1.875000000000000000, -1.201902961143720860 ) ) ;
#5155 = CARTESIAN_POINT ( 'NONE',  ( 3.750000000000000000, 13.75000000000000000, -3.500000000000000444 ) ) ;
#5156 = ORIENTED_EDGE ( 'NONE', *, *, #14209, .F. ) ;
#5157 = ADVANCED_FACE ( 'NONE', ( #12887 ), #856, .F. ) ;
#5158 = CARTESIAN_POINT ( 'NONE',  ( -7.111859124059414228, 1.750000000000027311, 17.30358917253076356 ) ) ;
#5159 = CARTESIAN_POINT ( 'NONE',  ( 2.651650429449552870, 0.6250000000000000000, -6.151650429449554203 ) ) ;
#5160 = CARTESIAN_POINT ( 'NONE',  ( 7.333250748047245970, 3.724583123210837066, -25.23076155689903288 ) ) ;
#5161 = FACE_OUTER_BOUND ( 'NONE', #10428, .T. ) ;
#5162 =( BOUNDED_CURVE ( )  B_SPLINE_CURVE ( 3, ( #2400, #12996, #14007, #7096 ),
 .UNSPECIFIED., .F., .F. ) 
 B_SPLINE_CURVE_WITH_KNOTS ( ( 4, 4 ),
 ( 1.145418132354773411, 1.513845819058956765 ),
 .UNSPECIFIED. ) 
 CURVE ( )  GEOMETRIC_REPRESENTATION_ITEM ( )  RATIONAL_B_SPLINE_CURVE ( ( 1.000000000000000000, 0.9887203717716437357, 0.9887203717716437357, 1.000000000000000000 ) ) 
 REPRESENTATION_ITEM ( '' )  );
#5163 = CARTESIAN_POINT ( 'NONE',  ( 0.000000000000000000, 2.000000000000000000, 0.2500000000000002220 ) ) ;
#5164 = APPROVAL_DATE_TIME ( #5242, #6528 ) ;
#5165 = CARTESIAN_POINT ( 'NONE',  ( -2.972530561760178269, 1.218752542932547250E-31, -135.1148407643974281 ) ) ;
#5166 = DIRECTION ( 'NONE',  ( 0.000000000000000000, -0.000000000000000000, -1.000000000000000000 ) ) ;
#5167 = PRODUCT_RELATED_PRODUCT_CATEGORY ( 'detail', '', ( #1532 ) ) ;
#5168 = EDGE_LOOP ( 'NONE', ( #14812, #6461, #7756, #10351 ) ) ;
#5169 = CARTESIAN_POINT ( 'NONE',  ( -1.346194077712559167, 8.437500000000000000, -6.749999999999999112 ) ) ;
#5170 = CARTESIAN_POINT ( 'NONE',  ( -8.953163619368993409, 1.337050190710010744, -104.6006781143766631 ) ) ;
#5171 = CARTESIAN_POINT ( 'NONE',  ( 2.298097038856279362, 12.87500000000000178, -1.201902961143720860 ) ) ;
#5172 = EDGE_CURVE ( 'NONE', #11237, #1120, #12444, .T. ) ;
#5173 = CARTESIAN_POINT ( 'NONE',  ( -3.249999999999999556, 11.75000000000000178, -3.500000000000000000 ) ) ;
#5174 = CARTESIAN_POINT ( 'NONE',  ( -5.826275610442698927, 15.00000000000000000, -101.5594179200140132 ) ) ;
#5175 = EDGE_CURVE ( 'NONE', #11904, #4807, #11379, .T. ) ;
#5176 = CARTESIAN_POINT ( 'NONE',  ( 0.000000000000000000, 1.000000000000000000, -0.2500000000000002220 ) ) ;
#5177 = EDGE_CURVE ( 'NONE', #3665, #14114, #5460, .T. ) ;
#5178 = CARTESIAN_POINT ( 'NONE',  ( 11.32016196459919755, 12.49999999999999822, -106.4092894470421271 ) ) ;
#5179 = CARTESIAN_POINT ( 'NONE',  ( -1.346194077712559389, 6.062500000000000000, -0.2500000000000002220 ) ) ;
#5180 = CARTESIAN_POINT ( 'NONE',  ( 3.749999999999998668, 6.187500000000001776, -5.053300858899108405 ) ) ;
#5181 = CARTESIAN_POINT ( 'NONE',  ( 2.651650429449553759, 7.875000000000000000, -0.8483495705504471296 ) ) ;
#5182 = LOCAL_TIME ( 12, 28, 20.00000000000000000, #8158 ) ;
#5183 = CARTESIAN_POINT ( 'NONE',  ( 0.2625675448779696275, 4.834017756466201021, 2.974107436473219845 ) ) ;
#5184 = CARTESIAN_POINT ( 'NONE',  ( -2.651650429449553314, 10.87499999999999822, -6.151650429449552426 ) ) ;
#5185 = CARTESIAN_POINT ( 'NONE',  ( 1.041519256436086005, 6.000000000000000000, -139.4527716894432956 ) ) ;
#5186 = AXIS2_PLACEMENT_3D ( 'NONE', #2920, #14609, #12416 ) ;
#5187 = PRODUCT_RELATED_PRODUCT_CATEGORY ( 'detail', '', ( #12881 ) ) ;
#5188 = CARTESIAN_POINT ( 'NONE',  ( 12.73368604874516485, 3.759190274397234521, -166.5778610917592175 ) ) ;
#5189 = DIRECTION ( 'NONE',  ( 0.000000000000000000, 1.000000000000000000, 0.000000000000000000 ) ) ;
#5190 = CARTESIAN_POINT ( 'NONE',  ( -4.492499072540820926, 5.000000000000000000, 2.611025101989610686 ) ) ;
#5191 = DIRECTION ( 'NONE',  ( -0.000000000000000000, 1.000000000000000000, -0.000000000000000000 ) ) ;
#5192 = FACE_OUTER_BOUND ( 'NONE', #4292, .T. ) ;
#5193 = CARTESIAN_POINT ( 'NONE',  ( -3.750000000000000000, 12.81250000000000178, -5.053300858899105741 ) ) ;
#5194 = ORIENTED_EDGE ( 'NONE', *, *, #5137, .T. ) ;
#5195 = CARTESIAN_POINT ( 'NONE',  ( 4.033098156699464809, 0.09438068890155107415, -1.663700395152567513 ) ) ;
#5196 = CARTESIAN_POINT ( 'NONE',  ( 7.995229681650333653, -1.921202954650397032, -34.56909192082981974 ) ) ;
#5197 = CARTESIAN_POINT ( 'NONE',  ( -3.749999999999999556, 8.187500000000000000, -1.946699141100892927 ) ) ;
#5198 = CARTESIAN_POINT ( 'NONE',  ( 3.749999999999998668, 8.187500000000000000, -5.053300858899108405 ) ) ;
#5199 = VECTOR ( 'NONE', #8829, 1000.000000000000114 ) ;
#5200 = CARTESIAN_POINT ( 'NONE',  ( -3.334719860237880695, 10.18881969361360085, -43.92205146497627055 ) ) ;
#5201 = VERTEX_POINT ( 'NONE', #15006 ) ;
#5202 = CARTESIAN_POINT ( 'NONE',  ( 1.346194077712561166, 10.43750000000000178, -0.2500000000000011102 ) ) ;
#5203 = CARTESIAN_POINT ( 'NONE',  ( -4.592425496802573972E-16, 8.500000000000000000, -7.249999999999999112 ) ) ;
#5204 = CARTESIAN_POINT ( 'NONE',  ( -66.67437826163231307, 15.00000000000000000, -172.5466827975835713 ) ) ;
#5205 = AXIS2_PLACEMENT_3D ( 'NONE', #6477, #14772, #5249 ) ;
#5206 = DIRECTION ( 'NONE',  ( 0.000000000000000000, -1.000000000000000000, 0.000000000000000000 ) ) ;
#5207 = DIRECTION ( 'NONE',  ( -0.02290662775272929094, -0.02291264298747154593, 0.9994750107913288328 ) ) ;
#5208 = CARTESIAN_POINT ( 'NONE',  ( -1.346194077712559389, 11.06250000000000000, -0.2500000000000002220 ) ) ;
#5209 = AXIS2_PLACEMENT_3D ( 'NONE', #6681, #4437, #816 ) ;
#5210 = DIRECTION ( 'NONE',  ( 0.000000000000000000, 0.000000000000000000, -1.000000000000000000 ) ) ;
#5211 = CIRCLE ( 'NONE', #5693, 2.999999999999999112 ) ;
#5212 = DIRECTION ( 'NONE',  ( 0.000000000000000000, 1.000000000000000000, 0.000000000000000000 ) ) ;
#5213 = CARTESIAN_POINT ( 'NONE',  ( 8.348030713307990069, 8.673617379884035472E-16, -112.8139498890285068 ) ) ;
#5214 = FACE_OUTER_BOUND ( 'NONE', #12931, .T. ) ;
#5215 = LINE ( 'NONE', #14659, #496 ) ;
#5216 = ORIENTED_EDGE ( 'NONE', *, *, #8855, .F. ) ;
#5217 = CARTESIAN_POINT ( 'NONE',  ( 8.941167358697452272, 11.11422854771078050, 2.597912425534024017 ) ) ;
#5218 = ADVANCED_BREP_SHAPE_REPRESENTATION ( '', ( #12454, #9419 ), #12893 ) ;
#5219 = DIRECTION ( 'NONE',  ( 0.000000000000000000, 0.000000000000000000, 1.000000000000000000 ) ) ;
#5220 = CARTESIAN_POINT ( 'NONE',  ( 2.651650429449553314, 12.37500000000000178, -0.8483495705504476847 ) ) ;
#5221 = CARTESIAN_POINT ( 'NONE',  ( -3.249999999999999112, 9.812500000000000000, -4.846194077712558723 ) ) ;
#5222 = CARTESIAN_POINT ( 'NONE',  ( -1.346194077712559167, 13.93750000000000000, -6.749999999999999112 ) ) ;
#5223 = VERTEX_POINT ( 'NONE', #5838 ) ;
#5224 = B_SPLINE_CURVE_WITH_KNOTS ( 'NONE', 3,
 ( #1200, #4908, #14274, #2599, #11938, #9707, #9474, #3674, #5072, #9787, #14200, #13109, #9623, #3603, #14441, #7134, #8305, #14356, #13033, #3755, #7298, #2440, #7766, #14899, #10015, #10087, #8699, #7608 ),
 .UNSPECIFIED., .F., .F.,
 ( 4, 2, 2, 2, 2, 2, 2, 2, 2, 2, 2, 2, 2, 4 ),
 ( 0.000000000000000000, 0.003096043757848191032, 0.006192087515696415023, 0.009288131273544638147, 0.01238417503139286301, 0.01393219691031695809, 0.01548021878924104797, 0.01702824066816514131, 0.01780225160762721054, 0.01857626254708927283, 0.02012428442601341128, 0.02167230630493754626, 0.02322032818386167777, 0.02476835006278580928 ),
 .UNSPECIFIED. ) ;
#5225 = CIRCLE ( 'NONE', #284, 2.499999999999999556 ) ;
#5226 = B_SPLINE_CURVE_WITH_KNOTS ( 'NONE', 3,
 ( #10879, #5165, #3003, #5318, #8554, #2693 ),
 .UNSPECIFIED., .F., .F.,
 ( 4, 2, 4 ),
 ( 0.000000000000000000, 0.008325297288147995647, 0.01665059457629599129 ),
 .UNSPECIFIED. ) ;
#5227 = CARTESIAN_POINT ( 'NONE',  ( 2.298097038856278473, 6.625000000000000000, -5.798097038856279362 ) ) ;
#5228 = CARTESIAN_POINT ( 'NONE',  ( 5.228075279701640099, 1.000000000000000000, -163.7939279834373849 ) ) ;
#5229 = CARTESIAN_POINT ( 'NONE',  ( -4.726777819131537051, 14.99999999979950083, -103.4097970346266777 ) ) ;
#5230 = DIRECTION ( 'NONE',  ( 0.000000000000000000, 0.000000000000000000, 1.000000000000000000 ) ) ;
#5231 = CARTESIAN_POINT ( 'NONE',  ( -16.94138229547581531, 5.000000000000000000, -154.2864167784019571 ) ) ;
#5232 = DATE_TIME_ROLE ( 'classification_date' ) ;
#5233 = FACE_OUTER_BOUND ( 'NONE', #10159, .T. ) ;
#5234 = ORIENTED_EDGE ( 'NONE', *, *, #728, .F. ) ;
#5235 = CARTESIAN_POINT ( 'NONE',  ( 1.346194077712558057, 0.5625000000000001110, -6.750000000000000000 ) ) ;
#5236 = CARTESIAN_POINT ( 'NONE',  ( 2.651650429449553759, 12.87500000000000178, -0.8483495705504471296 ) ) ;
#5237 = ORIENTED_EDGE ( 'NONE', *, *, #5908, .T. ) ;
#5238 = CARTESIAN_POINT ( 'NONE',  ( -1.553300858899106629, 2.062500000000000000, 0.2500000000000002220 ) ) ;
#5239 = CARTESIAN_POINT ( 'NONE',  ( 7.287561263328109717, 3.487951394471136446, -24.83885049245541410 ) ) ;
#5240 = CARTESIAN_POINT ( 'NONE',  ( 3.172663221847307646, 2.774810772982750251, 4.699280811759631860 ) ) ;
#5241 = CARTESIAN_POINT ( 'NONE',  ( 0.000000000000000000, 1.000000000000000000, -3.500000000000000000 ) ) ;
#5242 = DATE_AND_TIME ( #11039, #6464 ) ;
#5243 = EDGE_CURVE ( 'NONE', #5493, #9716, #14047, .T. ) ;
#5244 = CARTESIAN_POINT ( 'NONE',  ( -65.93966772342872673, 14.90901270607003504, -188.7849136839470248 ) ) ;
#5245 = DIRECTION ( 'NONE',  ( 0.000000000000000000, 0.000000000000000000, -1.000000000000000000 ) ) ;
#5246 = CC_DESIGN_APPROVAL ( #2654, ( #9258 ) ) ;
#5247 = ORIENTED_EDGE ( 'NONE', *, *, #4599, .F. ) ;
#5248 = CARTESIAN_POINT ( 'NONE',  ( -1.346194077712559167, 5.437500000000001776, -6.749999999999999112 ) ) ;
#5249 = DIRECTION ( 'NONE',  ( 0.6527336816407252051, 0.000000000000000000, -0.7575874476598356555 ) ) ;
#5250 = CARTESIAN_POINT ( 'NONE',  ( -3.980102097228897738E-16, 3.000000000000000444, -6.749999999999999112 ) ) ;
#5251 = CARTESIAN_POINT ( 'NONE',  ( -3.249999999999999112, 11.81250000000000178, -4.846194077712558723 ) ) ;
#5252 = PLANE ( 'NONE',  #71 ) ;
#5253 = DIRECTION ( 'NONE',  ( 0.000000000000000000, -1.000000000000000000, 0.000000000000000000 ) ) ;
#5254 = CARTESIAN_POINT ( 'NONE',  ( -3.249999999999999556, 4.187500000000000000, -2.153805922287440833 ) ) ;
#5255 = CARTESIAN_POINT ( 'NONE',  ( 3.749999999999998668, 5.187499999999999112, -5.053300858899108405 ) ) ;
#5256 = CARTESIAN_POINT ( 'NONE',  ( -2.651650429449552870, 11.12500000000000000, -0.8483495705504462414 ) ) ;
#5257 = CARTESIAN_POINT ( 'NONE',  ( -3.306254070109473808, 2.579293035051157368, -1.000000000000001332 ) ) ;
#5258 = CARTESIAN_POINT ( 'NONE',  ( -9.681086997240697656, 4.299422167715417409, -116.3713800322179992 ) ) ;
#5259 = CARTESIAN_POINT ( 'NONE',  ( -3.750000000000000000, 11.68749999999999822, -1.946699141100893149 ) ) ;
#5260 = CARTESIAN_POINT ( 'NONE',  ( 7.365467492728136278, 10.00000000000000533, -111.8544754347062309 ) ) ;
#5261 = CARTESIAN_POINT ( 'NONE',  ( 12.18930925058789860, 2.167092202807543000, -166.0723187315431915 ) ) ;
#5262 = EDGE_CURVE ( 'NONE', #13240, #9168, #6494, .T. ) ;
#5263 = EDGE_CURVE ( 'NONE', #5040, #5891, #9476, .T. ) ;
#5264 = CARTESIAN_POINT ( 'NONE',  ( 22.05734493763782211, 0.000000000000000000, 29.73364058993713499 ) ) ;
#5265 = CARTESIAN_POINT ( 'NONE',  ( -25.24054375344501722, 4.000000000000112799, -170.3561389648133400 ) ) ;
#5266 = CARTESIAN_POINT ( 'NONE',  ( -0.3732829694918258223, 2.850949024098341860E-47, -108.7490593617764318 ) ) ;
#5267 = UNCERTAINTY_MEASURE_WITH_UNIT (LENGTH_MEASURE( 1.000000000000000082E-05 ), #6124, 'distance_accuracy_value', 'NONE');
#5268 = CARTESIAN_POINT ( 'NONE',  ( -45.52432922703760454, 9.999999999999998224, -160.5926188986135799 ) ) ;
#5269 = CARTESIAN_POINT ( 'NONE',  ( -3.750000000000000000, 12.68750000000000000, -1.946699141100893149 ) ) ;
#5270 = VERTEX_POINT ( 'NONE', #6564 ) ;
#5271 = DIRECTION ( 'NONE',  ( -0.9961255586397055328, 0.000000000000000000, 0.08794243244722442510 ) ) ;
#5272 = CARTESIAN_POINT ( 'NONE',  ( 9.318502292199219994, 1.005413715383896456, -105.8229423371888345 ) ) ;
#5273 = CARTESIAN_POINT ( 'NONE',  ( -3.749999999999999556, 11.18749999999999822, -1.946699141100892927 ) ) ;
#5274 = CARTESIAN_POINT ( 'NONE',  ( -3.749999999999999556, 6.750000000000000888, -3.499999999999999112 ) ) ;
#5275 = CARTESIAN_POINT ( 'NONE',  ( -3.333303897718212117, 9.945529814085967146, -43.56314777000268634 ) ) ;
#5276 = CARTESIAN_POINT ( 'NONE',  ( -9.868623142791424385, 4.607815636209187993, -115.7530035201766765 ) ) ;
#5277 = CIRCLE ( 'NONE', #1568, 3.000000000000010214 ) ;
#5278 = CARTESIAN_POINT ( 'NONE',  ( -2.298097038856279362, 6.875000000000000000, -5.798097038856278473 ) ) ;
#5279 = VECTOR ( 'NONE', #10775, 1000.000000000000000 ) ;
#5280 = CARTESIAN_POINT ( 'NONE',  ( 2.651650429449552870, 0.1250000000000001110, -6.151650429449555091 ) ) ;
#5281 = DIRECTION ( 'NONE',  ( 0.9989498407774362043, 0.000000000000000000, 0.04581719776170026237 ) ) ;
#5282 = CARTESIAN_POINT ( 'NONE',  ( 0.9234955565201180550, 5.000000000000000888, -138.4305453062657421 ) ) ;
#5283 = DIRECTION ( 'NONE',  ( 1.000000000000000000, 0.000000000000000000, 0.000000000000000000 ) ) ;
#5284 = CARTESIAN_POINT ( 'NONE',  ( 3.249999999999999556, 13.75000000000000000, -3.500000000000000000 ) ) ;
#5285 = EDGE_CURVE ( 'NONE', #2585, #14605, #10267, .T. ) ;
#5286 = CARTESIAN_POINT ( 'NONE',  ( 7.753811188820757039, 2.743867526398027223, -39.64929316069591891 ) ) ;
#5287 = LINE ( 'NONE', #9999, #11458 ) ;
#5288 = CARTESIAN_POINT ( 'NONE',  ( 8.425472749221725621, 5.000000000000000888, -115.5475827924929035 ) ) ;
#5289 = AXIS2_PLACEMENT_3D ( 'NONE', #5577, #10292, #15029 ) ;
#5290 = DIRECTION ( 'NONE',  ( -0.9961255586397056438, 0.000000000000000000, 0.08794243244722428632 ) ) ;
#5291 = CIRCLE ( 'NONE', #10707, 1.000000000000000888 ) ;
#5292 = LINE ( 'NONE', #1810, #7133 ) ;
#5293 = ORIENTED_EDGE ( 'NONE', *, *, #834, .T. ) ;
#5294 = DIRECTION ( 'NONE',  ( 0.3072466363781645171, -0.8090169943749466741, -0.5010898195402013755 ) ) ;
#5295 = DIRECTION ( 'NONE',  ( 3.469446951953639038E-15, 0.000000000000000000, -1.000000000000000000 ) ) ;
#5296 = CARTESIAN_POINT ( 'NONE',  ( -3.749999999999999556, 12.75000000000000178, -3.499999999999999112 ) ) ;
#5297 = CARTESIAN_POINT ( 'NONE',  ( 3.249999999999999556, 11.25000000000000178, -3.500000000000000000 ) ) ;
#5298 = CARTESIAN_POINT ( 'NONE',  ( 3.249999999999999556, 14.25000000000000178, -3.500000000000000000 ) ) ;
#5299 = ORIENTED_EDGE ( 'NONE', *, *, #11781, .T. ) ;
#5300 = CARTESIAN_POINT ( 'NONE',  ( 2.298097038856279362, 9.875000000000000000, -1.201902961143720860 ) ) ;
#5301 = AXIS2_PLACEMENT_3D ( 'NONE', #1265, #7051, #11768 ) ;
#5302 = CARTESIAN_POINT ( 'NONE',  ( -14.94456014049648473, 7.499999999999991118, -95.36532121293905107 ) ) ;
#5303 = CARTESIAN_POINT ( 'NONE',  ( -7.135297789371368715, 14.04257511099845246, -104.0245404908031759 ) ) ;
#5304 = DIRECTION ( 'NONE',  ( 0.000000000000000000, 1.000000000000000000, 0.000000000000000000 ) ) ;
#5305 = CARTESIAN_POINT ( 'NONE',  ( -8.195495352953928503, 13.58490726914820002, -116.3141769265031655 ) ) ;
#5306 = APPROVAL_DATE_TIME ( #11172, #4690 ) ;
#5307 = DIRECTION ( 'NONE',  ( 0.000000000000000000, -1.000000000000000000, 0.000000000000000000 ) ) ;
#5308 = EDGE_LOOP ( 'NONE', ( #13248, #3625, #4137 ) ) ;
#5309 = CARTESIAN_POINT ( 'NONE',  ( 1.346194077712558057, 4.562500000000000888, -6.750000000000000000 ) ) ;
#5310 = CIRCLE ( 'NONE', #5544, 9.499999999999953815 ) ;
#5311 = CARTESIAN_POINT ( 'NONE',  ( 1.553300858899108849, 12.93750000000000000, 0.2499999999999993616 ) ) ;
#5312 = VERTEX_POINT ( 'NONE', #4028 ) ;
#5313 = CARTESIAN_POINT ( 'NONE',  ( -4.878690035801932723, 0.000000000000000000, -0.3860167444088152822 ) ) ;
#5314 = CARTESIAN_POINT ( 'NONE',  ( 2.651650429449552870, 1.625000000000000222, -6.151650429449554203 ) ) ;
#5315 = CARTESIAN_POINT ( 'NONE',  ( 0.1381806943969094426, 2.747451044191305591, 1.565175280801531121 ) ) ;
#5316 = CARTESIAN_POINT ( 'NONE',  ( 11.32016196458614488, 4.659658575830587068, -106.4092894464441486 ) ) ;
#5317 = PERSON_AND_ORGANIZATION ( #3176, #3020 ) ;
#5318 = CARTESIAN_POINT ( 'NONE',  ( 2.592859759274376064, 8.673617379884034486E-16, -128.9226664866425551 ) ) ;
#5319 = CARTESIAN_POINT ( 'NONE',  ( 26.71007981443201018, 5.000000000000000888, -136.8791680534710054 ) ) ;
#5320 = ORIENTED_EDGE ( 'NONE', *, *, #6964, .T. ) ;
#5321 = CARTESIAN_POINT ( 'NONE',  ( -2.298097038856278473, 9.125000000000000000, -1.201902961143720416 ) ) ;
#5322 = LINE ( 'NONE', #12278, #7147 ) ;
#5323 = CARTESIAN_POINT ( 'NONE',  ( 0.000000000000000000, 2.500000000000000000, -0.2500000000000002220 ) ) ;
#5324 = CARTESIAN_POINT ( 'NONE',  ( 1.346194077712561166, 10.43750000000000178, -0.2500000000000011102 ) ) ;
#5325 = CARTESIAN_POINT ( 'NONE',  ( -3.148647831469975955, 15.00000000000000000, -104.3063035292612142 ) ) ;
#5326 = DIRECTION ( 'NONE',  ( -0.6918711009959885860, -0.000000000000000000, -0.7220210382022110851 ) ) ;
#5327 = EDGE_CURVE ( 'NONE', #5060, #2896, #8908, .T. ) ;
#5328 = CARTESIAN_POINT ( 'NONE',  ( 0.000000000000000000, 5.000000000000000000, -0.2500000000000002220 ) ) ;
#5329 = CARTESIAN_POINT ( 'NONE',  ( -1.553300858899107073, 3.937500000000000444, -7.249999999999999112 ) ) ;
#5330 = CARTESIAN_POINT ( 'NONE',  ( -1.553300858899107073, 11.43750000000000000, -7.250000000000000000 ) ) ;
#5331 = CARTESIAN_POINT ( 'NONE',  ( -9.385448347264265578, 4.649823776045643342, -115.3551636530116866 ) ) ;
#5332 = CARTESIAN_POINT ( 'NONE',  ( 18.44985294524426322, -2.051692149507289097E-14, 26.15777747556343868 ) ) ;
#5333 = CARTESIAN_POINT ( 'NONE',  ( 3.750000000000000000, 11.31250000000000000, -1.946699141100892705 ) ) ;
#5334 = CARTESIAN_POINT ( 'NONE',  ( 4.337102815223837560, 14.99579250108048534, -0.6629991664209412550 ) ) ;
#5335 = CARTESIAN_POINT ( 'NONE',  ( -8.842600465860288139, -2.075239479414269894, -40.10276331981361864 ) ) ;
#5336 = CARTESIAN_POINT ( 'NONE',  ( -1.528156170053301510, 7.379999999999995453, -45.73714083922575213 ) ) ;
#5337 = CARTESIAN_POINT ( 'NONE',  ( -29.14779469708810566, 3.999999999999993783, -181.3194353810159498 ) ) ;
#5338 = CARTESIAN_POINT ( 'NONE',  ( 2.298097038856278473, 0.6250000000000000000, -5.798097038856279362 ) ) ;
#5339 = CARTESIAN_POINT ( 'NONE',  ( -34.50207410548875941, 15.00000000000000000, -151.1654763756944817 ) ) ;
#5340 = CARTESIAN_POINT ( 'NONE',  ( 3.749999999999999556, 14.25000000000000178, -3.500000000000000444 ) ) ;
#5341 = ORIENTED_EDGE ( 'NONE', *, *, #15218, .F. ) ;
#5342 = CARTESIAN_POINT ( 'NONE',  ( 8.673617379884035472E-16, 5.000000000000000888, -1.663700395152567513 ) ) ;
#5343 = DIRECTION ( 'NONE',  ( 0.000000000000000000, 0.000000000000000000, 1.000000000000000000 ) ) ;
#5344 = CARTESIAN_POINT ( 'NONE',  ( 2.651650429449553314, 10.37500000000000000, -0.8483495705504476847 ) ) ;
#5345 = CARTESIAN_POINT ( 'NONE',  ( 26.58801926426210116, 5.000000000000000888, -139.0072983920785532 ) ) ;
#5346 = B_SPLINE_CURVE_WITH_KNOTS ( 'NONE', 3,
 ( #6862, #10337, #7010, #62, #8096, #15158, #3613, #4474, #9337, #2309, #6936, #10567, #1071, #9184, #3537, #11575, #3313, #1210 ),
 .UNSPECIFIED., .F., .F.,
 ( 4, 2, 2, 2, 2, 2, 2, 2, 4 ),
 ( 2.290542279903411082E-17, 0.001058365784500584416, 0.002116731569001145848, 0.002645914461251426455, 0.003175097353501707496, 0.004233463138002267409, 0.005291828922502828624, 0.006350194707003389838, 0.008466926276004512267 ),
 .UNSPECIFIED. ) ;
#5347 = EDGE_CURVE ( 'NONE', #6217, #1578, #28, .T. ) ;
#5348 = CARTESIAN_POINT ( 'NONE',  ( -2.298097038856279362, 8.875000000000000000, -5.798097038856278473 ) ) ;
#5349 = EDGE_CURVE ( 'NONE', #4915, #1255, #626, .T. ) ;
#5350 = CARTESIAN_POINT ( 'NONE',  ( -31.08239538787591272, 9.999999999999998224, -156.3637655406869271 ) ) ;
#5351 = CARTESIAN_POINT ( 'NONE',  ( -2.651650429449552870, 12.12500000000000000, -0.8483495705504462414 ) ) ;
#5352 = CARTESIAN_POINT ( 'NONE',  ( 3.136841903360915396, 5.000000000000000888, -104.4936450199714955 ) ) ;
#5353 = DIRECTION ( 'NONE',  ( 0.000000000000000000, 1.000000000000000000, 0.000000000000000000 ) ) ;
#5354 = CARTESIAN_POINT ( 'NONE',  ( -1.346194077712559389, 12.43750000000000000, -6.749999999999999112 ) ) ;
#5355 = CARTESIAN_POINT ( 'NONE',  ( -25.82983890416511841, 15.00000000000000000, -142.4527639562402328 ) ) ;
#5356 = AXIS2_PLACEMENT_3D ( 'NONE', #12617, #3258, #15184 ) ;
#5357 = LINE ( 'NONE', #12618, #12708 ) ;
#5358 = CARTESIAN_POINT ( 'NONE',  ( 9.550372275008729872, 0.000000000000000000, -109.1178429856683181 ) ) ;
#5359 = CARTESIAN_POINT ( 'NONE',  ( 8.219148137446875779, 9.765288867732527697E-12, -129.9861206049809823 ) ) ;
#5360 = LINE ( 'NONE', #12389, #10634 ) ;
#5361 = EDGE_LOOP ( 'NONE', ( #8142, #6905, #351, #3905 ) ) ;
#5362 = CARTESIAN_POINT ( 'NONE',  ( 9.993646670323888870, 5.943472311793079221, -45.62742802061889336 ) ) ;
#5363 = CARTESIAN_POINT ( 'NONE',  ( -0.2500000000000000555, 5.000000000000000000, 1.500000000000000222 ) ) ;
#5364 = CARTESIAN_POINT ( 'NONE',  ( 1.553300858899108849, 1.937500000000000000, 0.2499999999999993616 ) ) ;
#5365 = CARTESIAN_POINT ( 'NONE',  ( -3.249999999999999112, 12.68750000000000178, -2.153805922287440833 ) ) ;
#5366 = CARTESIAN_POINT ( 'NONE',  ( 2.298097038856279362, 0.8750000000000000000, -1.201902961143720860 ) ) ;
#5367 = ORIENTED_EDGE ( 'NONE', *, *, #9328, .F. ) ;
#5368 = EDGE_CURVE ( 'NONE', #6054, #8964, #3730, .T. ) ;
#5369 = CARTESIAN_POINT ( 'NONE',  ( -3.249999999999999556, 11.18749999999999822, -2.153805922287440833 ) ) ;
#5370 = EDGE_CURVE ( 'NONE', #6769, #3728, #10387, .T. ) ;
#5371 = EDGE_CURVE ( 'NONE', #13242, #559, #697, .T. ) ;
#5372 = CARTESIAN_POINT ( 'NONE',  ( 9.969726460969127402, 12.69562161215808516, -44.88270096458933978 ) ) ;
#5373 = CARTESIAN_POINT ( 'NONE',  ( -7.195331454196918664, 13.84373920325294982, -104.6286638800799125 ) ) ;
#5374 = CARTESIAN_POINT ( 'NONE',  ( -25.37350819791483403, 4.000000000000000000, -209.1133945293850900 ) ) ;
#5375 = CARTESIAN_POINT ( 'NONE',  ( 26.73766085848595964, 6.000000000000000000, -138.7442440334353364 ) ) ;
#5376 = PERSON_AND_ORGANIZATION_ROLE ( 'classification_officer' ) ;
#5377 = CARTESIAN_POINT ( 'NONE',  ( 9.136110106120531427, 14.99999999999624833, -109.8557328640159483 ) ) ;
#5378 = CARTESIAN_POINT ( 'NONE',  ( 20.87131526946576443, 1.301042606982605321E-15, -138.9752963459259547 ) ) ;
#5379 = ORIENTED_EDGE ( 'NONE', *, *, #7026, .T. ) ;
#5380 = CARTESIAN_POINT ( 'NONE',  ( 1.346194077712558057, 6.562500000000000000, -6.750000000000000000 ) ) ;
#5381 = CARTESIAN_POINT ( 'NONE',  ( -8.671560925439079526, -2.743867526398025891, -35.09585054340071508 ) ) ;
#5382 = CARTESIAN_POINT ( 'NONE',  ( 3.750000000000000000, 2.312500000000000000, -1.946699141100892705 ) ) ;
#5383 = ORIENTED_EDGE ( 'NONE', *, *, #12030, .T. ) ;
#5384 = CARTESIAN_POINT ( 'NONE',  ( -4.234402844927150689, 15.00000000000000000, -117.4888040839639558 ) ) ;
#5385 = CARTESIAN_POINT ( 'NONE',  ( -2.651650429449552870, 1.125000000000000222, -0.8483495705504462414 ) ) ;
#5386 = CC_DESIGN_PERSON_AND_ORGANIZATION_ASSIGNMENT ( #10570, #12751, ( #8939 ) ) ;
#5387 = CARTESIAN_POINT ( 'NONE',  ( 7.553398589900353066, 3.720833046399418809, -21.52982307368431236 ) ) ;
#5388 = CARTESIAN_POINT ( 'NONE',  ( 3.215693626676934702, 3.859180552924430074, 5.079574387784768774 ) ) ;
#5389 = CARTESIAN_POINT ( 'NONE',  ( -1.553300858899106407, 1.062500000000000222, 0.2500000000000002220 ) ) ;
#5390 = COORDINATED_UNIVERSAL_TIME_OFFSET ( 0, 0, .AHEAD. ) ;
#5391 = CARTESIAN_POINT ( 'NONE',  ( 8.885817745189735106, 5.000000000000000000, -110.4710698842959573 ) ) ;
#5392 = DIRECTION ( 'NONE',  ( 0.000000000000000000, 0.000000000000000000, 1.000000000000000000 ) ) ;
#5393 = ORIENTED_EDGE ( 'NONE', *, *, #1537, .F. ) ;
#5394 = CARTESIAN_POINT ( 'NONE',  ( -68.22913373597590692, 10.00000000000000000, -203.2015853754454042 ) ) ;
#5395 = CARTESIAN_POINT ( 'NONE',  ( -3.249999999999999556, 2.750000000000000444, -3.500000000000000000 ) ) ;
#5396 = CARTESIAN_POINT ( 'NONE',  ( -3.249999999999999112, 12.81250000000000178, -4.846194077712558723 ) ) ;
#5397 = CARTESIAN_POINT ( 'NONE',  ( 10.93110029320957821, 13.31722294372111470, -107.0492663392355297 ) ) ;
#5398 = B_SPLINE_CURVE_WITH_KNOTS ( 'NONE', 3,
 ( #11643, #5613, #124, #8614, #2600, #6307, #6064, #13272, #9788, #14443, #13350, #3838, #1596, #7219, #11939, #13195, #5985, #14201, #4995, #2759, #2524, #7462, #9708, #7299, #12177, #10860, #2676, #1361, #11023, #13034, #13110, #10782, #440, #5148, #3604, #199 ),
 .UNSPECIFIED., .F., .F.,
 ( 4, 2, 2, 2, 2, 2, 2, 2, 2, 2, 2, 2, 2, 2, 2, 2, 2, 4 ),
 ( 2.775557561562891351E-17, 0.007532187987778461540, 0.01129828198166771443, 0.01506437597555696818, 0.02259656396333555722, 0.03012875195111415147, 0.03389484594500344339, 0.03577789294194813619, 0.03766093993889282898, 0.04142703393278219376, 0.04519312792667156548, 0.04707617492361626521, 0.04895922192056095801, 0.05272531591445035748, 0.05460836291139506415, 0.05649140990833977083, 0.05837445690528447056, 0.06025750390222917030 ),
 .UNSPECIFIED. ) ;
#5399 = CARTESIAN_POINT ( 'NONE',  ( 10.56872662651230854, 14.06121913168272108, -106.8383111373542107 ) ) ;
#5400 = CARTESIAN_POINT ( 'NONE',  ( -1.553300858899107073, 4.937500000000000000, -7.249999999999999112 ) ) ;
#5401 = CARTESIAN_POINT ( 'NONE',  ( 3.749999999999999112, 7.687500000000000000, -5.053300858899108405 ) ) ;
#5402 = CARTESIAN_POINT ( 'NONE',  ( 10.96001076296047394, 5.773884160794588105, -44.27064330819454341 ) ) ;
#5403 = ORIENTED_EDGE ( 'NONE', *, *, #14458, .T. ) ;
#5404 = CARTESIAN_POINT ( 'NONE',  ( -3.797998901586684628, 10.20017658455565623, -43.02000379425279419 ) ) ;
#5405 = CARTESIAN_POINT ( 'NONE',  ( -1.553300858899107073, 11.93750000000000178, -7.249999999999999112 ) ) ;
#5406 = LINE ( 'NONE', #10121, #9473 ) ;
#5407 = CARTESIAN_POINT ( 'NONE',  ( 8.807773658247754156, 15.00000000000000000, -105.8689255569352667 ) ) ;
#5408 = ADVANCED_FACE ( 'NONE', ( #14780, #2868 ), #6486, .F. ) ;
#5409 = CARTESIAN_POINT ( 'NONE',  ( 37.88191578704504536, 0.000000000000000000, 42.20832867525968624 ) ) ;
#5410 = EDGE_LOOP ( 'NONE', ( #13278, #8200, #2284, #7286 ) ) ;
#5411 = CARTESIAN_POINT ( 'NONE',  ( -27.13173129639779901, 4.000000000000835776, -174.9559605998265681 ) ) ;
#5412 = CARTESIAN_POINT ( 'NONE',  ( -44.50300032302160957, 9.999999999999998224, -159.8141794074082327 ) ) ;
#5413 = CARTESIAN_POINT ( 'NONE',  ( 3.249999999999998224, 0.3125000000000002220, -2.153805922287439945 ) ) ;
#5414 = ORIENTED_EDGE ( 'NONE', *, *, #9298, .F. ) ;
#5415 = FACE_OUTER_BOUND ( 'NONE', #12407, .T. ) ;
#5416 = CARTESIAN_POINT ( 'NONE',  ( 5.000000000000000000, 5.000000000000000888, -100.6237003951525679 ) ) ;
#5417 = DIRECTION ( 'NONE',  ( 0.000000000000000000, 1.734723475976805517E-15, -1.000000000000000000 ) ) ;
#5418 = CARTESIAN_POINT ( 'NONE',  ( -19.41689661852894844, 8.673617379884033500E-16, -190.2656566201660837 ) ) ;
#5419 = CARTESIAN_POINT ( 'NONE',  ( 4.892302586675363330, 0.000000000000000000, -102.5092683516849661 ) ) ;
#5420 = CARTESIAN_POINT ( 'NONE',  ( -3.249999999999999112, 7.687500000000000000, -2.153805922287440833 ) ) ;
#5421 = FACE_OUTER_BOUND ( 'NONE', #11361, .T. ) ;
#5422 = CARTESIAN_POINT ( 'NONE',  ( 1.553300858899108849, 14.93750000000000178, 0.2499999999999993616 ) ) ;
#5423 = CARTESIAN_POINT ( 'NONE',  ( -1.500000000000000000, 4.500000000000000888, 0.2500000000000002220 ) ) ;
#5424 = CARTESIAN_POINT ( 'NONE',  ( -5.309262520577839872, 13.36526483154179523, -125.0911079416483176 ) ) ;
#5425 = CARTESIAN_POINT ( 'NONE',  ( -3.249999999999999556, 12.25000000000000000, -3.499999999999999556 ) ) ;
#5426 = CARTESIAN_POINT ( 'NONE',  ( 4.716951098700680411, 2.490287375297123962, -44.10818225254242009 ) ) ;
#5427 = LOCAL_TIME ( 12, 28, 20.00000000000000000, #741 ) ;
#5428 = EDGE_CURVE ( 'NONE', #6005, #8015, #10344, .T. ) ;
#5429 = CARTESIAN_POINT ( 'NONE',  ( 10.97171279554003043, 8.773889247172311556, -44.61149169061435060 ) ) ;
#5430 = CARTESIAN_POINT ( 'NONE',  ( 2.298097038856278473, 8.625000000000000000, -5.798097038856279362 ) ) ;
#5431 = CIRCLE ( 'NONE', #13348, 3.500000000000003109 ) ;
#5432 = DIRECTION ( 'NONE',  ( -0.000000000000000000, -1.000000000000000000, -0.000000000000000000 ) ) ;
#5433 = EDGE_LOOP ( 'NONE', ( #10752, #7466 ) ) ;
#5434 = CARTESIAN_POINT ( 'NONE',  ( 8.983524629129894024, 12.48417253965678064, 0.6570725777486732255 ) ) ;
#5435 = CARTESIAN_POINT ( 'NONE',  ( 29.15191114725999455, 8.773889247172311556, -41.21400910903738435 ) ) ;
#5436 = CARTESIAN_POINT ( 'NONE',  ( 3.750000000000000000, 1.750000000000000000, -3.500000000000000444 ) ) ;
#5437 = CARTESIAN_POINT ( 'NONE',  ( -3.750000000000000000, 0.6875000000000000000, -1.946699141100893149 ) ) ;
#5438 = CARTESIAN_POINT ( 'NONE',  ( 2.298097038856278029, 14.12500000000000000, -5.798097038856279362 ) ) ;
#5439 = ORIENTED_EDGE ( 'NONE', *, *, #11506, .F. ) ;
#5440 = CARTESIAN_POINT ( 'NONE',  ( 3.249999999999999112, 9.812500000000000000, -2.153805922287439945 ) ) ;
#5441 = CC_DESIGN_APPROVAL ( #2152, ( #3971 ) ) ;
#5442 = CARTESIAN_POINT ( 'NONE',  ( 10.01611035499524682, 11.63253765721051636, -45.55947799121552322 ) ) ;
#5443 = CIRCLE ( 'NONE', #6682, 1.000000000000000888 ) ;
#5444 = CIRCLE ( 'NONE', #3719, 4.000000000000002665 ) ;
#5445 = CARTESIAN_POINT ( 'NONE',  ( -6.583754373576919505, 14.38465807378985950, -103.8663350565541492 ) ) ;
#5446 = DIRECTION ( 'NONE',  ( -1.000000000000000000, 0.000000000000000000, 0.000000000000000000 ) ) ;
#5447 = CARTESIAN_POINT ( 'NONE',  ( -7.687033461059231243, 13.90392860197237823, -116.8257989789342730 ) ) ;
#5448 = EDGE_CURVE ( 'NONE', #5038, #3740, #14858, .T. ) ;
#5449 = CARTESIAN_POINT ( 'NONE',  ( 6.854384957879182672, 15.00000000000000000, -108.8103024308010589 ) ) ;
#5450 = FACE_OUTER_BOUND ( 'NONE', #955, .T. ) ;
#5451 = EDGE_CURVE ( 'NONE', #5655, #1404, #7585, .T. ) ;
#5452 = CARTESIAN_POINT ( 'NONE',  ( 23.60198427277999755, 0.4374050601044401354, -138.3407798013068657 ) ) ;
#5453 = ADVANCED_FACE ( 'NONE', ( #12360 ), #7074, .F. ) ;
#5454 = TOROIDAL_SURFACE ( 'NONE', #6924, 9.800000000000267164, 5.000000000000000000 ) ;
#5455 = ORIENTED_EDGE ( 'NONE', *, *, #5428, .T. ) ;
#5456 = AXIS2_PLACEMENT_3D ( 'NONE', #10847, #2427, #2510 ) ;
#5457 = CARTESIAN_POINT ( 'NONE',  ( -1.346194077712559389, 3.062500000000000000, -0.2500000000000002220 ) ) ;
#5458 = CARTESIAN_POINT ( 'NONE',  ( -30.17038736920199682, 4.000000000000000888, -186.2979594716615566 ) ) ;
#5459 = CARTESIAN_POINT ( 'NONE',  ( 1.553300858899109516, 0.4375000000000000555, 0.2499999999999993616 ) ) ;
#5460 = CIRCLE ( 'NONE', #14354, 3.500000000000003109 ) ;
#5461 = VERTEX_POINT ( 'NONE', #9556 ) ;
#5462 = CARTESIAN_POINT ( 'NONE',  ( -8.031487215395609169, 13.41211965017131469, -115.9574366882090146 ) ) ;
#5463 = LINE ( 'NONE', #14913, #7005 ) ;
#5464 = CARTESIAN_POINT ( 'NONE',  ( -3.750000000000000000, 4.250000000000000000, -3.499999999999999112 ) ) ;
#5465 = AXIS2_PLACEMENT_3D ( 'NONE', #5624, #5920, #10646 ) ;
#5466 = CARTESIAN_POINT ( 'NONE',  ( 7.429120998017664235, 4.464394614690160523, -25.99568145149812182 ) ) ;
#5467 = CARTESIAN_POINT ( 'NONE',  ( 0.03998412334521193184, 8.673617379884035472E-16, 0.4529009045602688799 ) ) ;
#5468 = CARTESIAN_POINT ( 'NONE',  ( 1.553300858899105963, 1.562500000000000000, -7.250000000000000000 ) ) ;
#5469 = SHAPE_DEFINITION_REPRESENTATION ( #11752, #9314 ) ;
#5470 = CARTESIAN_POINT ( 'NONE',  ( 10.02605224556585384, 4.999999999999999112, -108.3589403638364530 ) ) ;
#5471 = ADVANCED_FACE ( 'NONE', ( #8778 ), #8315, .F. ) ;
#5472 = VERTEX_POINT ( 'NONE', #3995 ) ;
#5473 = DIRECTION ( 'NONE',  ( -0.000000000000000000, 1.000000000000000000, -0.000000000000000000 ) ) ;
#5474 = CARTESIAN_POINT ( 'NONE',  ( -3.249999999999999112, 4.812500000000000000, -4.846194077712558723 ) ) ;
#5475 = AXIS2_PLACEMENT_3D ( 'NONE', #3443, #13903, #1059 ) ;
#5476 = DIRECTION ( 'NONE',  ( 0.000000000000000000, 0.000000000000000000, 1.000000000000000000 ) ) ;
#5477 =( BOUNDED_SURFACE ( )  B_SPLINE_SURFACE ( 3, 2, ( 
 ( #2864, #12282, #1692 ),
 ( #9963, #11121, #540 ),
 ( #13534, #14929, #13754 ),
 ( #12505, #770, #9029 ),
 ( #1923, #6636, #3149 ),
 ( #11343, #5478, #10196 ),
 ( #4326, #10826, #9591 ),
 ( #95, #2490, #5041 ),
 ( #244, #6035, #14405 ),
 ( #3803, #11755, #14319 ),
 ( #4808, #3885, #9759 ),
 ( #328, #12061, #4959 ),
 ( #3723, #11826, #10678 ),
 ( #1250, #5956, #7184 ),
 ( #13005, #9674, #8348 ),
 ( #9522, #1175, #8508 ),
 ( #5876, #13243, #2722 ),
 ( #7271, #4733, #8428 ),
 ( #4879, #10596, #14487 ),
 ( #2410, #11985, #7348 ),
 ( #14172, #13161, #2646 ),
 ( #1479, #6194, #3575 ),
 ( #14243, #2570, #3645 ),
 ( #11907, #13074, #17 ),
 ( #10910, #1331, #6113 ),
 ( #1408, #8584, #13317 ),
 ( #9444, #10755, #172 ),
 ( #8277, #7106, #13870 ),
 ( #12856, #1179, #8127 ),
 ( #6893, #12629, #5659 ),
 ( #5588, #4588, #6823 ),
 ( #9295, #5738, #5813 ) ),
 .UNSPECIFIED., .F., .F., .T. ) 
 B_SPLINE_SURFACE_WITH_KNOTS ( ( 4, 2, 2, 2, 2, 2, 2, 2, 2, 2, 2, 2, 2, 2, 2, 4 ),
 ( 3, 3 ),
 ( 0.000000000000000000, 0.003626821300828501123, 0.007253642601657002247, 0.009067053252071253025, 0.01088046390248550294, 0.01450728520331400449, 0.01632069585372825440, 0.01813410650414250605, 0.01904081182934962840, 0.01994751715455675423, 0.02176092780497100587, 0.02357433845538525752, 0.02448104378059238334, 0.02538774910579950916, 0.02720115975621376081, 0.02901457040662800899 ),
 ( 0.000000000000000000, 1.000000000000000000 ),
 .UNSPECIFIED. ) 
 GEOMETRIC_REPRESENTATION_ITEM ( )  RATIONAL_B_SPLINE_SURFACE ( (
 ( 1.000000000000000000, 0.7071067811865475727, 1.000000000000000000),
 ( 1.000000000000000000, 0.7071067811865475727, 1.000000000000000000),
 ( 1.000000000000000000, 0.7071067811865475727, 1.000000000000000000),
 ( 1.000000000000000000, 0.7071067811865475727, 1.000000000000000000),
 ( 1.000000000000000000, 0.7071067811865475727, 1.000000000000000000),
 ( 1.000000000000000000, 0.7071067811865475727, 1.000000000000000000),
 ( 1.000000000000000000, 0.7071067811865475727, 1.000000000000000000),
 ( 1.000000000000000000, 0.7071067811865475727, 1.000000000000000000),
 ( 1.000000000000000000, 0.7071067811865475727, 1.000000000000000000),
 ( 1.000000000000000000, 0.7071067811865475727, 1.000000000000000000),
 ( 1.000000000000000000, 0.7071067811865475727, 1.000000000000000000),
 ( 1.000000000000000000, 0.7071067811865475727, 1.000000000000000000),
 ( 1.000000000000000000, 0.7071067811865476838, 1.000000000000000000),
 ( 1.000000000000000000, 0.7071067811865476838, 1.000000000000000000),
 ( 1.000000000000000000, 0.7071067811865474617, 1.000000000000000000),
 ( 1.000000000000000000, 0.7071067811865474617, 1.000000000000000000),
 ( 1.000000000000000000, 0.7071067811865475727, 1.000000000000000000),
 ( 1.000000000000000000, 0.7071067811865475727, 1.000000000000000000),
 ( 1.000000000000000000, 0.7071067811865475727, 1.000000000000000000),
 ( 1.000000000000000000, 0.7071067811865475727, 1.000000000000000000),
 ( 1.000000000000000000, 0.7071067811865475727, 1.000000000000000000),
 ( 1.000000000000000000, 0.7071067811865475727, 1.000000000000000000),
 ( 1.000000000000000000, 0.7071067811865475727, 1.000000000000000000),
 ( 1.000000000000000000, 0.7071067811865475727, 1.000000000000000000),
 ( 1.000000000000000000, 0.7071067811865485719, 1.000000000000000000),
 ( 1.000000000000000000, 0.7071067811865485719, 1.000000000000000000),
 ( 1.000000000000000000, 0.7071067811865475727, 1.000000000000000000),
 ( 1.000000000000000000, 0.7071067811865475727, 1.000000000000000000),
 ( 1.000000000000000000, 0.7071067811865460184, 1.000000000000000000),
 ( 1.000000000000000000, 0.7071067811865460184, 1.000000000000000000),
 ( 1.000000000000000000, 0.7071067811865460184, 1.000000000000000000),
 ( 1.000000000000000000, 0.7071067811865460184, 1.000000000000000000) ) ) 
 REPRESENTATION_ITEM ( '' )  SURFACE ( )  );
#5478 = CARTESIAN_POINT ( 'NONE',  ( -7.754603562414723150, -2.363702682127649382E-12, -121.4663199873584034 ) ) ;
#5479 = CARTESIAN_POINT ( 'NONE',  ( 3.749999999999999112, 5.312500000000000000, -1.946699141100893149 ) ) ;
#5480 = CARTESIAN_POINT ( 'NONE',  ( 2.651650429449553759, 12.87500000000000178, -0.8483495705504471296 ) ) ;
#5481 = CARTESIAN_POINT ( 'NONE',  ( -3.055795963278728600, 2.474488745542203549, -1.000000000000011990 ) ) ;
#5482 = DIRECTION ( 'NONE',  ( -0.000000000000000000, 1.000000000000000000, -0.000000000000000000 ) ) ;
#5483 = CARTESIAN_POINT ( 'NONE',  ( 1.346194077712560944, 7.937500000000000888, -0.2500000000000010547 ) ) ;
#5484 = CARTESIAN_POINT ( 'NONE',  ( 3.749999999999999112, 12.18750000000000178, -5.053300858899108405 ) ) ;
#5485 = CARTESIAN_POINT ( 'NONE',  ( 4.882278757662108504, 14.90393508816177714, -1.535399676672468905 ) ) ;
#5486 = CARTESIAN_POINT ( 'NONE',  ( 8.513076393186699065, 14.99999999999999822, -106.2110621154036494 ) ) ;
#5487 = CARTESIAN_POINT ( 'NONE',  ( 11.04730217088350663, 5.000000000000000888, -107.1178495010082941 ) ) ;
#5488 = ORIENTED_EDGE ( 'NONE', *, *, #14414, .T. ) ;
#5489 = CARTESIAN_POINT ( 'NONE',  ( -27.18350272990648264, 1.080414591133489251E-12, -177.5702011201350103 ) ) ;
#5490 = DIRECTION ( 'NONE',  ( 0.000000000000000000, 0.000000000000000000, -1.000000000000000000 ) ) ;
#5491 = CARTESIAN_POINT ( 'NONE',  ( -33.72825374957025701, 15.00000000000000000, -151.1581928109187345 ) ) ;
#5492 = CARTESIAN_POINT ( 'NONE',  ( 3.249999999999998224, 4.187500000000000888, -4.846194077712561388 ) ) ;
#5493 = VERTEX_POINT ( 'NONE', #12972 ) ;
#5494 = CARTESIAN_POINT ( 'NONE',  ( -9.110371329266945040, 9.999999999999998224, -123.5182978443285720 ) ) ;
#5495 = CARTESIAN_POINT ( 'NONE',  ( 7.000000000000000888, 15.00000000000000000, -1.663700395152567513 ) ) ;
#5496 = CARTESIAN_POINT ( 'NONE',  ( -33.91109452335874153, 5.000000000000000000, -156.1716796081737471 ) ) ;
#5497 = CARTESIAN_POINT ( 'NONE',  ( -9.868623143902821582, 5.000000000000003553, -115.7530035192419433 ) ) ;
#5498 = CARTESIAN_POINT ( 'NONE',  ( -3.980102097228897738E-16, 10.00000000000000000, -6.749999999999999112 ) ) ;
#5499 = DIRECTION ( 'NONE',  ( 1.000000000000000000, 0.000000000000000000, 0.000000000000000000 ) ) ;
#5500 = CARTESIAN_POINT ( 'NONE',  ( 0.000000000000000000, 15.00000000000000000, 0.2500000000000002220 ) ) ;
#5501 = CARTESIAN_POINT ( 'NONE',  ( -67.29661116483785577, 15.00000000000001243, -205.0278900928574615 ) ) ;
#5502 = CARTESIAN_POINT ( 'NONE',  ( -8.631701571668326523, 11.65889702651062443, -105.3772359608016984 ) ) ;
#5503 = CARTESIAN_POINT ( 'NONE',  ( -3.249999999999999556, 11.31249999999999822, -4.846194077712557835 ) ) ;
#5504 = CARTESIAN_POINT ( 'NONE',  ( -0.5793326530874193248, 2.075239479414269894, -43.47630266472464911 ) ) ;
#5505 = CARTESIAN_POINT ( 'NONE',  ( 4.856804767890306351, 14.90536770052033866, -1.840041787218210878 ) ) ;
#5506 = CARTESIAN_POINT ( 'NONE',  ( -3.249999999999999556, 10.18750000000000000, -2.153805922287440833 ) ) ;
#5507 = CARTESIAN_POINT ( 'NONE',  ( -4.994618032138967045, 8.673617379884035472E-16, -137.1639743028343048 ) ) ;
#5508 = DIRECTION ( 'NONE',  ( 0.000000000000000000, -0.000000000000000000, -1.000000000000000000 ) ) ;
#5509 = ORIENTED_EDGE ( 'NONE', *, *, #13763, .T. ) ;
#5510 = CARTESIAN_POINT ( 'NONE',  ( 26.04203104729492679, -1.082694418179886911E-15, 69.41411580402544246 ) ) ;
#5511 = CARTESIAN_POINT ( 'NONE',  ( -22.63089125489394604, 3.999999999999999112, -204.5592954525788514 ) ) ;
#5512 = CARTESIAN_POINT ( 'NONE',  ( -3.750000000000000000, 14.81250000000000355, -5.053300858899105741 ) ) ;
#5513 = AXIS2_PLACEMENT_3D ( 'NONE', #9855, #14588, #2834 ) ;
#5514 = CARTESIAN_POINT ( 'NONE',  ( -2.651650429449552870, 1.874999999999999778, -6.151650429449552426 ) ) ;
#5515 = CARTESIAN_POINT ( 'NONE',  ( -3.249999999999999556, 0.1875000000000000278, -2.153805922287440833 ) ) ;
#5516 = VERTEX_POINT ( 'NONE', #5228 ) ;
#5517 = CARTESIAN_POINT ( 'NONE',  ( 3.249999999999998668, 12.68750000000000178, -4.846194077712560500 ) ) ;
#5518 = ADVANCED_FACE ( 'NONE', ( #2904 ), #5692, .T. ) ;
#5519 = DIRECTION ( 'NONE',  ( -0.08794243244722425856, -0.000000000000000000, -0.9961255586397054218 ) ) ;
#5520 = DIRECTION ( 'NONE',  ( 0.000000000000000000, 0.000000000000000000, -1.000000000000000000 ) ) ;
#5521 =( LENGTH_UNIT ( ) NAMED_UNIT ( * ) SI_UNIT ( .MILLI., .METRE. ) );
#5522 = CARTESIAN_POINT ( 'NONE',  ( -6.465967782645682504, 14.60719871297730243, -116.8537262797239151 ) ) ;
#5523 = TOROIDAL_SURFACE ( 'NONE', #10468, 3.750000000000003553, 0.5000000000000000000 ) ;
#5524 = DATE_AND_TIME ( #513, #5427 ) ;
#5525 = CIRCLE ( 'NONE', #3300, 1.750000000000001554 ) ;
#5526 = CARTESIAN_POINT ( 'NONE',  ( 7.622624992407810218, 15.00000000000000000, -121.2625470869670181 ) ) ;
#5527 = CARTESIAN_POINT ( 'NONE',  ( 3.891364641103949307, 14.90536770052033688, -1.768596708628434211 ) ) ;
#5528 = CARTESIAN_POINT ( 'NONE',  ( 26.11837629089787782, 1.928122897211196340, -137.7354575184153589 ) ) ;
#5529 = VERTEX_POINT ( 'NONE', #132 ) ;
#5530 = CARTESIAN_POINT ( 'NONE',  ( 3.249999999999999112, 2.812500000000000000, -2.153805922287439945 ) ) ;
#5531 = CARTESIAN_POINT ( 'NONE',  ( -3.219147294323990938, -2.743867526398025891, -0.6706657213131048678 ) ) ;
#5532 = CARTESIAN_POINT ( 'NONE',  ( 3.749999999999999556, 2.249999999999999556, -3.500000000000000444 ) ) ;
#5533 = ORIENTED_EDGE ( 'NONE', *, *, #837, .T. ) ;
#5534 = CARTESIAN_POINT ( 'NONE',  ( -7.548446295636298764, 13.85765414864760459, -116.1647996692329485 ) ) ;
#5535 = CIRCLE ( 'NONE', #7509, 0.4999999999999726885 ) ;
#5536 = CARTESIAN_POINT ( 'NONE',  ( 6.321352278304661176, 5.000000000000000888, -106.5183844524637635 ) ) ;
#5537 = CARTESIAN_POINT ( 'NONE',  ( -3.749999999999999556, 6.187500000000000888, -1.946699141100892927 ) ) ;
#5538 = EDGE_CURVE ( 'NONE', #13371, #14267, #3222, .T. ) ;
#5539 = CARTESIAN_POINT ( 'NONE',  ( -25.29096338392381327, 1.168513153268224259E-15, -199.8929960699789206 ) ) ;
#5540 = CARTESIAN_POINT ( 'NONE',  ( 0.4428117151818120600, 2.348215632956504262, 5.015736486741213085 ) ) ;
#5541 = CARTESIAN_POINT ( 'NONE',  ( -1.553300858899106407, 3.062500000000000000, 0.2500000000000002220 ) ) ;
#5542 = PERSON_AND_ORGANIZATION ( #3176, #3020 ) ;
#5543 = CARTESIAN_POINT ( 'NONE',  ( 9.971950858281140029, 8.773889247172311556, -44.63331069169930032 ) ) ;
#5544 = AXIS2_PLACEMENT_3D ( 'NONE', #2357, #6906, #14189 ) ;
#5545 = DIRECTION ( 'NONE',  ( 0.000000000000000000, 0.000000000000000000, 1.000000000000000000 ) ) ;
#5546 = EDGE_LOOP ( 'NONE', ( #7367, #7542, #5079, #1478, #10297, #3418 ) ) ;
#5547 = CARTESIAN_POINT ( 'NONE',  ( -3.980102097228897738E-16, 4.000000000000000000, -6.749999999999999112 ) ) ;
#5548 = CARTESIAN_POINT ( 'NONE',  ( 9.391154601535028235, 14.93751321453985170, -106.1795410437272551 ) ) ;
#5549 = CARTESIAN_POINT ( 'NONE',  ( -1.553300858899107073, 10.93750000000000355, -7.249999999999999112 ) ) ;
#5550 = EDGE_CURVE ( 'NONE', #14561, #7952, #436, .T. ) ;
#5551 = CARTESIAN_POINT ( 'NONE',  ( 3.750000000000000000, 13.75000000000000000, -3.500000000000000444 ) ) ;
#5552 = CARTESIAN_POINT ( 'NONE',  ( -5.525175898872280555, 0.1455664706284490462, -116.9935625178451772 ) ) ;
#5553 = ORIENTED_EDGE ( 'NONE', *, *, #6104, .T. ) ;
#5554 = CARTESIAN_POINT ( 'NONE',  ( -8.926802767664643312, 2.381696043666894358, -116.5496838980187562 ) ) ;
#5555 = CARTESIAN_POINT ( 'NONE',  ( -3.249999999999999556, 0.7500000000000001110, -3.500000000000000000 ) ) ;
#5556 = DIRECTION ( 'NONE',  ( -0.000000000000000000, 1.000000000000000000, -0.000000000000000000 ) ) ;
#5557 = PERSON_AND_ORGANIZATION_ROLE ( 'classification_officer' ) ;
#5558 = CARTESIAN_POINT ( 'NONE',  ( 5.856634129115241727, 14.99999999999999822, -112.7529454488145859 ) ) ;
#5559 = CARTESIAN_POINT ( 'NONE',  ( 7.190027994173562753, 7.321094445766561876, -30.38850508759179192 ) ) ;
#5560 = VERTEX_POINT ( 'NONE', #14281 ) ;
#5561 = CARTESIAN_POINT ( 'NONE',  ( -25.72606948156193951, 8.673617379884035472E-16, -194.7310816857908549 ) ) ;
#5562 = FACE_OUTER_BOUND ( 'NONE', #3432, .T. ) ;
#5563 = CARTESIAN_POINT ( 'NONE',  ( -41.27834176923248322, 9.999999999999998224, -157.9203444102009826 ) ) ;
#5564 = CARTESIAN_POINT ( 'NONE',  ( 0.000000000000000000, 4.499999999999999112, -0.2500000000000002220 ) ) ;
#5565 = EDGE_LOOP ( 'NONE', ( #1109, #10058, #2763, #15297, #7614, #9528, #6051, #1928 ) ) ;
#5566 = CARTESIAN_POINT ( 'NONE',  ( -0.4453226528549816265, -2.225540348348185052E-17, -1.000000000000000000 ) ) ;
#5567 = CARTESIAN_POINT ( 'NONE',  ( 5.228075279701640099, 1.000000000000000000, -165.7939279834373849 ) ) ;
#5568 = LINE ( 'NONE', #10284, #2573 ) ;
#5569 = CARTESIAN_POINT ( 'NONE',  ( -3.980102097228897245E-16, 10.50000000000000000, -6.749999999999999112 ) ) ;
#5570 = CARTESIAN_POINT ( 'NONE',  ( 8.937327444046795577, 10.65305643749201181, 2.773860008794248433 ) ) ;
#5571 = CARTESIAN_POINT ( 'NONE',  ( -8.199037228201154548, 5.000000000000000888, -114.3845095685560835 ) ) ;
#5572 = CARTESIAN_POINT ( 'NONE',  ( -1.346194077712559167, 11.93750000000000178, -6.749999999999999112 ) ) ;
#5573 = CARTESIAN_POINT ( 'NONE',  ( -33.91109452337774854, 10.00000000000000178, -156.1716796081737471 ) ) ;
#5574 = CARTESIAN_POINT ( 'NONE',  ( 2.651650429449552870, 14.62500000000000000, -6.151650429449554203 ) ) ;
#5575 = CARTESIAN_POINT ( 'NONE',  ( -65.53364736412717662, 15.00000000000000000, -205.7441351029432894 ) ) ;
#5576 = CARTESIAN_POINT ( 'NONE',  ( -8.223364455376053428, 12.56334999322341517, -105.1585554315304165 ) ) ;
#5577 = CARTESIAN_POINT ( 'NONE',  ( 0.000000000000000000, 3.061616997868383018E-17, 0.2500000000000002220 ) ) ;
#5578 = CARTESIAN_POINT ( 'NONE',  ( 22.25537508876543313, 0.1342633940746081334, -138.4925780178333810 ) ) ;
#5579 = LINE ( 'NONE', #4204, #2837 ) ;
#5580 = CARTESIAN_POINT ( 'NONE',  ( -3.249999999999999556, 7.187500000000000000, -2.153805922287440833 ) ) ;
#5581 = CARTESIAN_POINT ( 'NONE',  ( 2.530298019944474675, 0.000000000000000000, 0.2330448234422078380 ) ) ;
#5582 = LINE ( 'NONE', #13864, #7646 ) ;
#5583 = ORIENTED_EDGE ( 'NONE', *, *, #3653, .F. ) ;
#5584 = ORIENTED_EDGE ( 'NONE', *, *, #4696, .T. ) ;
#5585 = FACE_BOUND ( 'NONE', #2917, .T. ) ;
#5586 = CARTESIAN_POINT ( 'NONE',  ( -2.651650429449553314, 0.3750000000000000555, -6.151650429449552426 ) ) ;
#5587 = CARTESIAN_POINT ( 'NONE',  ( -2.298097038856279362, 13.87500000000000178, -5.798097038856278473 ) ) ;
#5588 = CARTESIAN_POINT ( 'NONE',  ( -6.941963816496072859, 4.336808689942017736E-16, -103.8778697715490011 ) ) ;
#5589 = ORIENTED_EDGE ( 'NONE', *, *, #797, .T. ) ;
#5590 = CARTESIAN_POINT ( 'NONE',  ( 0.000000000000000000, 12.00000000000000000, -0.2500000000000002220 ) ) ;
#5591 = CARTESIAN_POINT ( 'NONE',  ( -3.315923205871632362, 9.650666666666662508, -43.24506100211545601 ) ) ;
#5592 = CARTESIAN_POINT ( 'NONE',  ( -3.980102097228897245E-16, 7.500000000000000000, -6.749999999999999112 ) ) ;
#5593 = CARTESIAN_POINT ( 'NONE',  ( -8.718986484435074402, 11.36792136375515483, -105.4248486380225813 ) ) ;
#5594 = COORDINATED_UNIVERSAL_TIME_OFFSET ( 0, 0, .AHEAD. ) ;
#5595 = CARTESIAN_POINT ( 'NONE',  ( 9.781725384962639325, 15.00000000000000000, -108.7377634488996136 ) ) ;
#5596 = FACE_OUTER_BOUND ( 'NONE', #10773, .T. ) ;
#5597 = ADVANCED_FACE ( 'NONE', ( #60 ), #7146, .T. ) ;
#5598 = VERTEX_POINT ( 'NONE', #3681 ) ;
#5599 = CARTESIAN_POINT ( 'NONE',  ( 26.02337256472977245, 2.644888176801018176, -137.1336233889525715 ) ) ;
#5600 = CARTESIAN_POINT ( 'NONE',  ( 1.346194077712560944, 11.93750000000000000, -0.2500000000000011102 ) ) ;
#5601 = ORIENTED_EDGE ( 'NONE', *, *, #4888, .F. ) ;
#5602 = VERTEX_POINT ( 'NONE', #1143 ) ;
#5603 = CARTESIAN_POINT ( 'NONE',  ( 1.346194077712560944, 2.937500000000000444, -0.2500000000000010547 ) ) ;
#5604 = FACE_OUTER_BOUND ( 'NONE', #12033, .T. ) ;
#5605 = CARTESIAN_POINT ( 'NONE',  ( -3.749999999999999556, 1.750000000000000222, -3.499999999999999112 ) ) ;
#5606 = CARTESIAN_POINT ( 'NONE',  ( -3.249999999999999112, 6.687500000000000888, -2.153805922287440833 ) ) ;
#5607 = ORIENTED_EDGE ( 'NONE', *, *, #12030, .F. ) ;
#5608 = DIRECTION ( 'NONE',  ( 0.000000000000000000, -1.000000000000000000, 0.000000000000000000 ) ) ;
#5609 = DIRECTION ( 'NONE',  ( 0.000000000000000000, 0.000000000000000000, -1.000000000000000000 ) ) ;
#5610 = APPLICATION_CONTEXT ( 'configuration controlled 3d designs of mechanical parts and assemblies' ) ;
#5611 = CARTESIAN_POINT ( 'NONE',  ( -4.592425496802573972E-16, 6.500000000000000888, -7.249999999999999112 ) ) ;
#5612 = CARTESIAN_POINT ( 'NONE',  ( -24.89144347233892773, 2.130041083117732992, -207.5316459546360193 ) ) ;
#5613 = CARTESIAN_POINT ( 'NONE',  ( -63.01211225522952475, 9.999999999999998224, -201.0953633257875026 ) ) ;
#5614 = SHAPE_DEFINITION_REPRESENTATION ( #10650, #4394 ) ;
#5615 = DIRECTION ( 'NONE',  ( -0.000000000000000000, -1.000000000000000000, -0.000000000000000000 ) ) ;
#5616 = EDGE_LOOP ( 'NONE', ( #2848, #9033, #656, #2342 ) ) ;
#5617 = ADVANCED_FACE ( 'NONE', ( #1664 ), #2000, .T. ) ;
#5618 = CARTESIAN_POINT ( 'NONE',  ( -3.980102097228897738E-16, 7.000000000000000000, -6.749999999999999112 ) ) ;
#5619 = CARTESIAN_POINT ( 'NONE',  ( -5.082498805844316792, 10.00000000000000178, -111.2070015758558839 ) ) ;
#5620 = CARTESIAN_POINT ( 'NONE',  ( 0.000000000000000000, 8.500000000000000000, 0.2499999999999998057 ) ) ;
#5621 = CARTESIAN_POINT ( 'NONE',  ( 2.651650429449553759, 14.87500000000000178, -0.8483495705504471296 ) ) ;
#5622 = CARTESIAN_POINT ( 'NONE',  ( -64.80788720177807249, 14.99074302883816756, -184.1356180242662788 ) ) ;
#5623 = EDGE_LOOP ( 'NONE', ( #1753, #8664, #2270, #6234 ) ) ;
#5624 = CARTESIAN_POINT ( 'NONE',  ( 9.044950117654433797, 4.000000000000000000, -141.4826476090360643 ) ) ;
#5625 = CARTESIAN_POINT ( 'NONE',  ( -3.749999999999999556, 13.75000000000000000, -3.499999999999999112 ) ) ;
#5626 = CARTESIAN_POINT ( 'NONE',  ( 10.97846948146473700, 13.76924748112251784, -106.3333921311819523 ) ) ;
#5627 =( NAMED_UNIT ( * ) SI_UNIT ( $, .STERADIAN. ) SOLID_ANGLE_UNIT ( ) );
#5628 = FACE_BOUND ( 'NONE', #15115, .T. ) ;
#5629 = ORIENTED_EDGE ( 'NONE', *, *, #3372, .T. ) ;
#5630 = EDGE_CURVE ( 'NONE', #6631, #4876, #14603, .T. ) ;
#5631 = CARTESIAN_POINT ( 'NONE',  ( -24.98726638638703790, 3.999999999999993783, -209.5206582725076032 ) ) ;
#5632 = CARTESIAN_POINT ( 'NONE',  ( -3.980102097228897245E-16, 0.5000000000000000000, -6.749999999999999112 ) ) ;
#5633 = ADVANCED_FACE ( 'NONE', ( #14591 ), #4756, .F. ) ;
#5634 = CARTESIAN_POINT ( 'NONE',  ( -62.68280523401330129, 14.99999999999469225, -198.2448752127326088 ) ) ;
#5635 = ADVANCED_FACE ( 'NONE', ( #2376 ), #5917, .F. ) ;
#5636 = CARTESIAN_POINT ( 'NONE',  ( 2.298097038856279362, 1.375000000000000000, -1.201902961143720860 ) ) ;
#5637 = ORIENTED_EDGE ( 'NONE', *, *, #11002, .T. ) ;
#5638 = CARTESIAN_POINT ( 'NONE',  ( 1.237310451418919932, -2.473751543678972542, -1.000000000000001332 ) ) ;
#5639 = CARTESIAN_POINT ( 'NONE',  ( -0.2500000000000000555, 5.000000000000000000, 0.2500000000000002220 ) ) ;
#5640 = CARTESIAN_POINT ( 'NONE',  ( 2.304446043347688100, 8.673617379884041389E-16, -168.0449129170526419 ) ) ;
#5641 = CARTESIAN_POINT ( 'NONE',  ( -1.030030361949073603, 5.000000000000000888, -105.0143096064271901 ) ) ;
#5642 = CARTESIAN_POINT ( 'NONE',  ( -1.346194077712558945, 10.56250000000000355, -0.2500000000000002220 ) ) ;
#5643 = DIRECTION ( 'NONE',  ( 0.000000000000000000, 1.000000000000000000, 0.000000000000000000 ) ) ;
#5644 = CARTESIAN_POINT ( 'NONE',  ( 3.750000000000000000, 2.312500000000000000, -1.946699141100892705 ) ) ;
#5645 = CARTESIAN_POINT ( 'NONE',  ( 3.230086971182892785, 10.25843542224570193, 5.208283727272518426 ) ) ;
#5646 = CARTESIAN_POINT ( 'NONE',  ( -6.790153584124027475, 9.999999999999998224, -124.9643354754709748 ) ) ;
#5647 =( BOUNDED_CURVE ( )  B_SPLINE_CURVE ( 3, ( #13691, #5185, #9896, #6568 ),
 .UNSPECIFIED., .F., .F. ) 
 B_SPLINE_CURVE_WITH_KNOTS ( ( 4, 4 ),
 ( 2.234491175284466280, 2.237794841200465790 ),
 .UNSPECIFIED. ) 
 CURVE ( )  GEOMETRIC_REPRESENTATION_ITEM ( )  RATIONAL_B_SPLINE_CURVE ( ( 1.000000000000000000, 0.9999990904828330862, 0.9999990904828330862, 1.000000000000000000 ) ) 
 REPRESENTATION_ITEM ( '' )  );
#5648 = CARTESIAN_POINT ( 'NONE',  ( -10.85850957030563713, 10.00000000000000178, -125.6943677036881866 ) ) ;
#5649 = CARTESIAN_POINT ( 'NONE',  ( -3.665378489062163236, 0.000000000000000000, 4.733462801983808532 ) ) ;
#5650 = CARTESIAN_POINT ( 'NONE',  ( -3.249999999999999556, 10.31250000000000000, -4.846194077712557835 ) ) ;
#5651 = FACE_OUTER_BOUND ( 'NONE', #5063, .T. ) ;
#5652 = DIRECTION ( 'NONE',  ( -0.000000000000000000, -1.000000000000000000, -0.000000000000000000 ) ) ;
#5653 = ORIENTED_EDGE ( 'NONE', *, *, #12446, .T. ) ;
#5654 = CC_DESIGN_DATE_AND_TIME_ASSIGNMENT ( #10327, #11563, ( #8872 ) ) ;
#5655 = VERTEX_POINT ( 'NONE', #15044 ) ;
#5656 = CARTESIAN_POINT ( 'NONE',  ( 2.735681601764421877, 0.000000000000000000, -172.9928595839035665 ) ) ;
#5657 = CARTESIAN_POINT ( 'NONE',  ( -3.750000000000000000, 2.250000000000000444, -3.499999999999999112 ) ) ;
#5658 = CARTESIAN_POINT ( 'NONE',  ( 0.000000000000000000, 13.50000000000000355, -0.2500000000000002220 ) ) ;
#5659 = CARTESIAN_POINT ( 'NONE',  ( -8.225432057776796313, 2.500000000000000444, -106.0978137656049824 ) ) ;
#5660 = EDGE_LOOP ( 'NONE', ( #4435, #10787, #8373, #1173 ) ) ;
#5661 = CARTESIAN_POINT ( 'NONE',  ( 1.346194077712558057, 14.56250000000000000, -6.750000000000000000 ) ) ;
#5662 = FACE_OUTER_BOUND ( 'NONE', #6817, .T. ) ;
#5663 = CC_DESIGN_APPROVAL ( #15090, ( #5003 ) ) ;
#5664 = CARTESIAN_POINT ( 'NONE',  ( -8.948682078903175352, 11.69044914887355979, -104.5711183077397948 ) ) ;
#5665 = AXIS2_PLACEMENT_3D ( 'NONE', #11452, #6512, #9058 ) ;
#5666 = CARTESIAN_POINT ( 'NONE',  ( 1.346194077712560944, 2.937500000000000444, -0.2500000000000010547 ) ) ;
#5667 = AXIS2_PLACEMENT_3D ( 'NONE', #12561, #4597, #9306 ) ;
#5668 = APPROVAL_STATUS ( 'not_yet_approved' ) ;
#5669 = CYLINDRICAL_SURFACE ( 'NONE', #14949, 2.000000000000001776 ) ;
#5670 = CARTESIAN_POINT ( 'NONE',  ( -6.885999823355373195, 14.39196139387547468, -116.9934166929402295 ) ) ;
#5671 = ORIENTED_EDGE ( 'NONE', *, *, #9512, .F. ) ;
#5672 = CARTESIAN_POINT ( 'NONE',  ( 27.42902907614759656, 4.089980352809128306, -137.4133472663777127 ) ) ;
#5673 = CARTESIAN_POINT ( 'NONE',  ( 1.346194077712558279, 12.56250000000000000, -6.750000000000000000 ) ) ;
#5674 = VERTEX_POINT ( 'NONE', #6533 ) ;
#5675 = ORIENTED_EDGE ( 'NONE', *, *, #5285, .F. ) ;
#5676 = CARTESIAN_POINT ( 'NONE',  ( 0.000000000000000000, 11.50000000000000000, 0.2500000000000002220 ) ) ;
#5677 = CARTESIAN_POINT ( 'NONE',  ( -8.289881740238502772, -2.529993217055221510, -35.21986562831451550 ) ) ;
#5678 = CARTESIAN_POINT ( 'NONE',  ( -4.592425496802573972E-16, 1.000000000000000000, -7.250000000000000000 ) ) ;
#5679 = CARTESIAN_POINT ( 'NONE',  ( -2.298097038856279362, 6.875000000000000000, -5.798097038856278473 ) ) ;
#5680 = VERTEX_POINT ( 'NONE', #4218 ) ;
#5681 = ORGANIZATION ( 'NAUO-ORG3', 'UNSPECIFIED', 'UNSPECIFIED' ) ;
#5682 = DIRECTION ( 'NONE',  ( 0.02181900108494707821, 0.000000000000000000, -0.9997619372588931741 ) ) ;
#5683 = CARTESIAN_POINT ( 'NONE',  ( 2.298097038856278473, 2.625000000000000000, -5.798097038856279362 ) ) ;
#5684 = CIRCLE ( 'NONE', #3965, 0.4999999999999726885 ) ;
#5685 = CARTESIAN_POINT ( 'NONE',  ( 1.553300858899108849, 5.937500000000000000, 0.2499999999999993616 ) ) ;
#5686 = CARTESIAN_POINT ( 'NONE',  ( -25.47867862103529646, 0.2061871876987354246, -202.7017271924692068 ) ) ;
#5687 = CARTESIAN_POINT ( 'NONE',  ( -11.94594212905470343, 10.00000000000000533, -150.3828439890653215 ) ) ;
#5688 = APPROVAL_DATE_TIME ( #3606, #4538 ) ;
#5689 = VECTOR ( 'NONE', #12079, 1000.000000000000000 ) ;
#5690 = CARTESIAN_POINT ( 'NONE',  ( 8.316464637237423574, 5.000000000000000000, -114.4073620934065048 ) ) ;
#5691 = VECTOR ( 'NONE', #4641, 1000.000000000000000 ) ;
#5692 = TOROIDAL_SURFACE ( 'NONE', #9891, 4.000000000000000000, 1.000000000000000000 ) ;
#5693 = AXIS2_PLACEMENT_3D ( 'NONE', #7790, #8797, #10032 ) ;
#5694 = B_SPLINE_CURVE_WITH_KNOTS ( 'NONE', 3,
 ( #15079, #5780, #8246, #15303, #4554, #8317, #13043, #10501, #11725, #4626, #2453, #14060 ),
 .UNSPECIFIED., .F., .F.,
 ( 4, 2, 2, 2, 2, 4 ),
 ( 2.168404344971008868E-18, 0.003032381943411205719, 0.006064763886822409703, 0.01212952777364481594, 0.01819429166046722390, 0.02425905554728963187 ),
 .UNSPECIFIED. ) ;
#5695 = ORIENTED_EDGE ( 'NONE', *, *, #3541, .F. ) ;
#5696 = CARTESIAN_POINT ( 'NONE',  ( 1.346194077712558279, 9.062500000000003553, -6.750000000000000888 ) ) ;
#5697 = FACE_OUTER_BOUND ( 'NONE', #10906, .T. ) ;
#5698 = AXIS2_PLACEMENT_3D ( 'NONE', #7377, #282, #1439 ) ;
#5699 = CARTESIAN_POINT ( 'NONE',  ( -2.651650429449552870, 8.875000000000000000, -6.151650429449552426 ) ) ;
#5700 = CARTESIAN_POINT ( 'NONE',  ( 3.749999999999999112, 14.68750000000000178, -5.053300858899108405 ) ) ;
#5701 = EDGE_CURVE ( 'NONE', #9864, #5223, #12399, .T. ) ;
#5702 = CARTESIAN_POINT ( 'NONE',  ( -66.40912117502934109, 14.82863921643819261, -191.0993814215748330 ) ) ;
#5703 = CARTESIAN_POINT ( 'NONE',  ( 0.2499999999999999445, 4.500000000000000888, -1.499999999999999778 ) ) ;
#5704 = CARTESIAN_POINT ( 'NONE',  ( -2.651650429449553314, 13.87500000000000178, -6.151650429449552426 ) ) ;
#5705 = CARTESIAN_POINT ( 'NONE',  ( -4.273407437632543271, 4.336808689942017243E-16, -107.1048060010029417 ) ) ;
#5706 = APPROVAL_ROLE ( '' ) ;
#5707 = PRODUCT_DEFINITION_SHAPE ( 'NONE', 'NONE',  #10487 ) ;
#5708 = CARTESIAN_POINT ( 'NONE',  ( -3.782526895735879524, 9.999999999999998224, -42.84475209785865246 ) ) ;
#5709 = ORIENTED_EDGE ( 'NONE', *, *, #9382, .T. ) ;
#5710 = PLANE ( 'NONE',  #2094 ) ;
#5711 = CARTESIAN_POINT ( 'NONE',  ( 0.000000000000000000, 2.000000000000000000, -0.2500000000000002220 ) ) ;
#5712 = CARTESIAN_POINT ( 'NONE',  ( -56.77487962284654088, 15.00000000000000000, -165.9012238629486262 ) ) ;
#5713 = CC_DESIGN_DATE_AND_TIME_ASSIGNMENT ( #3072, #4242, ( #9187 ) ) ;
#5714 = CARTESIAN_POINT ( 'NONE',  ( 1.346194077712561166, 1.437500000000000000, -0.2500000000000011102 ) ) ;
#5715 = ORIENTED_EDGE ( 'NONE', *, *, #1112, .T. ) ;
#5716 = CARTESIAN_POINT ( 'NONE',  ( 0.7644969749118040170, 5.000000000000000000, -138.4027240657576101 ) ) ;
#5717 = CARTESIAN_POINT ( 'NONE',  ( -25.31996789051264685, 0.02318398216220063368, -200.1489047904456129 ) ) ;
#5718 = CARTESIAN_POINT ( 'NONE',  ( 8.904552045041942421, 13.48516601183745500, 4.275651785405313099 ) ) ;
#5719 = CARTESIAN_POINT ( 'NONE',  ( 0.000000000000000000, 8.673617379884035472E-16, -100.6237003951525679 ) ) ;
#5720 = CARTESIAN_POINT ( 'NONE',  ( 3.249999999999998224, 12.18750000000000178, -4.846194077712561388 ) ) ;
#5721 = AXIS2_PLACEMENT_3D ( 'NONE', #12156, #3317, #4477 ) ;
#5722 = CARTESIAN_POINT ( 'NONE',  ( -0.3766621274091713767, 0.2975415354274087432, -7.146945437571386783 ) ) ;
#5723 = CARTESIAN_POINT ( 'NONE',  ( 1.553300858899109516, 0.4375000000000000555, 0.2499999999999993616 ) ) ;
#5724 = CARTESIAN_POINT ( 'NONE',  ( 6.089666224640344794, 15.00000000000000000, -124.6062682140657074 ) ) ;
#5725 = ADVANCED_FACE ( 'NONE', ( #11318 ), #3000, .F. ) ;
#5726 = CARTESIAN_POINT ( 'NONE',  ( -6.198501765558289911, 14.51381462227466201, -104.1424196585592057 ) ) ;
#5727 = CARTESIAN_POINT ( 'NONE',  ( 1.004809442601927394, 6.000000000000000000, -139.4752805618705622 ) ) ;
#5728 = CARTESIAN_POINT ( 'NONE',  ( -4.373225680752619304, 0.000000000000000000, 27.28944397070847927 ) ) ;
#5729 = CARTESIAN_POINT ( 'NONE',  ( 2.298097038856279362, 6.875000000000000000, -1.201902961143720860 ) ) ;
#5730 = CARTESIAN_POINT ( 'NONE',  ( 1.855481649321463200, 15.00000000000000000, -35.83830032691797385 ) ) ;
#5731 = DIRECTION ( 'NONE',  ( 0.000000000000000000, -1.000000000000000000, 0.000000000000000000 ) ) ;
#5732 = CC_DESIGN_APPROVAL ( #6183, ( #8443 ) ) ;
#5733 = ORIENTED_EDGE ( 'NONE', *, *, #9666, .F. ) ;
#5734 = ORIENTED_EDGE ( 'NONE', *, *, #7044, .T. ) ;
#5735 = CARTESIAN_POINT ( 'NONE',  ( -12.84530548741220990, -1.035315611211759139E-11, -188.5128586801774020 ) ) ;
#5736 = CARTESIAN_POINT ( 'NONE',  ( -3.749999999999999556, 6.187500000000000888, -1.946699141100892927 ) ) ;
#5737 = CARTESIAN_POINT ( 'NONE',  ( -1.553300858899107073, 1.937500000000000222, -7.249999999999999112 ) ) ;
#5738 = CARTESIAN_POINT ( 'NONE',  ( -9.000077715877313977, -1.040834085586084099E-14, -105.4229635846035222 ) ) ;
#5739 = VERTEX_POINT ( 'NONE', #8847 ) ;
#5740 = AXIS2_PLACEMENT_3D ( 'NONE', #12393, #14967, #6525 ) ;
#5741 = CARTESIAN_POINT ( 'NONE',  ( 1.346194077712560944, 14.93750000000000178, -0.2500000000000010547 ) ) ;
#5742 = DIRECTION ( 'NONE',  ( -0.000000000000000000, -1.000000000000000000, -0.000000000000000000 ) ) ;
#5743 = ADVANCED_FACE ( 'NONE', ( #1740 ), #12554, .T. ) ;
#5744 = DIRECTION ( 'NONE',  ( -0.000000000000000000, -1.000000000000000000, -0.000000000000000000 ) ) ;
#5745 = CARTESIAN_POINT ( 'NONE',  ( -3.249999999999999556, 2.187500000000000444, -2.153805922287440833 ) ) ;
#5746 = CALENDAR_DATE ( 2026, 8, 10 ) ;
#5747 = CARTESIAN_POINT ( 'NONE',  ( 0.5944212552585367293, 15.00000000000000000, -138.5540974747773930 ) ) ;
#5748 = FACE_OUTER_BOUND ( 'NONE', #10800, .T. ) ;
#5749 = ORIENTED_EDGE ( 'NONE', *, *, #3737, .T. ) ;
#5750 = PERSON ( 'NAUO-PER1', 'UNSPECIFIED', 'UNSPECIFIED', ('UNSPECIFIED'), ('UNSPECIFIED'), ('UNSPECIFIED') ) ;
#5751 = AXIS2_PLACEMENT_3D ( 'NONE', #6150, #13282, #14527 ) ;
#5752 = CARTESIAN_POINT ( 'NONE',  ( 1.831246893856133928, -2.490287375297125294, -1.000000000000000888 ) ) ;
#5753 = CARTESIAN_POINT ( 'NONE',  ( -1.346194077712558945, 10.06250000000000000, -0.2500000000000002220 ) ) ;
#5754 = ORIENTED_EDGE ( 'NONE', *, *, #4053, .T. ) ;
#5755 = ORIENTED_EDGE ( 'NONE', *, *, #7602, .T. ) ;
#5756 = CARTESIAN_POINT ( 'NONE',  ( 3.749999999999999556, 8.250000000000000000, -3.500000000000000444 ) ) ;
#5757 = DIRECTION ( 'NONE',  ( 0.000000000000000000, 1.000000000000000000, 0.000000000000000000 ) ) ;
#5758 = CARTESIAN_POINT ( 'NONE',  ( 1.553300858899105963, 7.062500000000000888, -7.250000000000000888 ) ) ;
#5759 = CARTESIAN_POINT ( 'NONE',  ( -3.249999999999999112, 7.812500000000000000, -4.846194077712558723 ) ) ;
#5760 = ORIENTED_EDGE ( 'NONE', *, *, #552, .T. ) ;
#5761 = CARTESIAN_POINT ( 'NONE',  ( 0.000000000000000000, 5.000000000000000000, -3.500000000000000000 ) ) ;
#5762 = CARTESIAN_POINT ( 'NONE',  ( 1.346194077712560944, 2.937500000000000444, -0.2500000000000010547 ) ) ;
#5763 = CARTESIAN_POINT ( 'NONE',  ( 3.749999999999999112, 7.812500000000000000, -1.946699141100892039 ) ) ;
#5764 = AXIS2_PLACEMENT_3D ( 'NONE', #9986, #2952, #7738 ) ;
#5765 = VECTOR ( 'NONE', #1861, 1000.000000000000000 ) ;
#5766 = CARTESIAN_POINT ( 'NONE',  ( -25.65051852152078737, 1.581731481231831049, -206.7883074467665097 ) ) ;
#5767 = LINE ( 'NONE', #10326, #14633 ) ;
#5768 = PERSON_AND_ORGANIZATION ( #3176, #3020 ) ;
#5769 = CARTESIAN_POINT ( 'NONE',  ( 6.436143463598921421, 5.000000000000000888, 2.800833825385760090 ) ) ;
#5770 = VERTEX_POINT ( 'NONE', #6451 ) ;
#5771 = AXIS2_PLACEMENT_3D ( 'NONE', #13379, #9886, #12493 ) ;
#5772 = AXIS2_PLACEMENT_3D ( 'NONE', #712, #9118, #3247 ) ;
#5773 = CARTESIAN_POINT ( 'NONE',  ( 3.249999999999998224, 8.312500000000003553, -2.153805922287439945 ) ) ;
#5774 = CARTESIAN_POINT ( 'NONE',  ( -10.29275726619094478, 1.020558061026469510, -34.56909192082969895 ) ) ;
#5775 = CARTESIAN_POINT ( 'NONE',  ( 3.749999999999998668, 10.18750000000000533, -5.053300858899108405 ) ) ;
#5776 = CARTESIAN_POINT ( 'NONE',  ( -3.750000000000000000, 12.18750000000000000, -1.946699141100892927 ) ) ;
#5777 = B_SPLINE_CURVE_WITH_KNOTS ( 'NONE', 3,
 ( #13239, #92, #7180, #4875, #8344, #5952, #9587, #9360, #6108, #5806, #12929, #168, #10527, #9519, #3799, #2486, #3572, #10751, #13, #10821, #8504, #2406, #3642, #9441, #14169, #13002, #2566, #1402, #11903, #6968 ),
 .UNSPECIFIED., .F., .F.,
 ( 4, 2, 2, 2, 2, 2, 2, 2, 2, 2, 2, 2, 2, 2, 4 ),
 ( 1.734723475976807094E-18, 0.0008039673220171474803, 0.001607934644034293226, 0.002411901966051438646, 0.003215869288068584717, 0.004823803932102929334, 0.006431738576137275253, 0.008039673220171619436, 0.009647607864205964487, 0.01286347715227465285, 0.01607934644034334642, 0.01929521572841203653, 0.02251108501648072663, 0.02411901966051507862, 0.02572695430454942367 ),
 .UNSPECIFIED. ) ;
#5778 = CARTESIAN_POINT ( 'NONE',  ( 3.249999999999999112, 11.81249999999999822, -2.153805922287439945 ) ) ;
#5779 = CARTESIAN_POINT ( 'NONE',  ( -64.23600185951367791, 13.34030093836066300, -200.8190070947437391 ) ) ;
#5780 = CARTESIAN_POINT ( 'NONE',  ( 0.6118422199237436576, 5.000000000000000888, -137.1181811292527470 ) ) ;
#5781 = CARTESIAN_POINT ( 'NONE',  ( 3.749999999999999112, 14.18750000000000178, -5.053300858899108405 ) ) ;
#5782 = DIRECTION ( 'NONE',  ( 1.000000000000000000, 0.000000000000000000, -0.000000000000000000 ) ) ;
#5783 = CALENDAR_DATE ( 2026, 8, 10 ) ;
#5784 = CARTESIAN_POINT ( 'NONE',  ( 26.30339064689345463, 0.000000000000000000, 68.98786334397659914 ) ) ;
#5785 = ORIENTED_EDGE ( 'NONE', *, *, #14546, .T. ) ;
#5786 = CARTESIAN_POINT ( 'NONE',  ( -25.78198310901690959, 3.999999999999627853, -208.7111422138455907 ) ) ;
#5787 = CARTESIAN_POINT ( 'NONE',  ( 3.249999999999999112, 4.812500000000000888, -2.153805922287439945 ) ) ;
#5788 = CARTESIAN_POINT ( 'NONE',  ( -63.24671589544670525, 15.00000000000000000, -204.0178512890850584 ) ) ;
#5789 = EDGE_CURVE ( 'NONE', #4779, #9239, #13726, .T. ) ;
#5790 = CARTESIAN_POINT ( 'NONE',  ( -3.249999999999999112, 2.687500000000000888, -2.153805922287440833 ) ) ;
#5791 = EDGE_LOOP ( 'NONE', ( #8068, #7684 ) ) ;
#5792 = CARTESIAN_POINT ( 'NONE',  ( -10.46704385831657902, 0.000000000000000000, -128.9524512386204549 ) ) ;
#5793 = CARTESIAN_POINT ( 'NONE',  ( -25.42939282183900573, 4.000000000000000000, -209.0516719515502473 ) ) ;
#5794 = CARTESIAN_POINT ( 'NONE',  ( 8.955009189050604945, 14.88563060951957340, 1.963670047743441449 ) ) ;
#5795 = DIRECTION ( 'NONE',  ( 0.02181900108494707127, 0.000000000000000000, -0.9997619372588931741 ) ) ;
#5796 = CARTESIAN_POINT ( 'NONE',  ( -1.346194077712559167, 13.93750000000000000, -6.749999999999999112 ) ) ;
#5797 = CARTESIAN_POINT ( 'NONE',  ( 20.84482309861724048, -1.169407659665303564E-12, -149.6621754078184665 ) ) ;
#5798 = CARTESIAN_POINT ( 'NONE',  ( 2.651650429449554203, 2.375000000000000000, -0.8483495705504471296 ) ) ;
#5799 = CYLINDRICAL_SURFACE ( 'NONE', #4245, 6.000000000000002665 ) ;
#5800 = CARTESIAN_POINT ( 'NONE',  ( -4.212126835263352298, 10.36695148008834266, -47.83691020068690847 ) ) ;
#5801 = CARTESIAN_POINT ( 'NONE',  ( 24.19680568221177452, 0.8824476403469397878, -137.8004069206694453 ) ) ;
#5802 = CARTESIAN_POINT ( 'NONE',  ( -1.873266413721881296, 0.000000000000000000, 1.481691765633328828 ) ) ;
#5803 = CARTESIAN_POINT ( 'NONE',  ( -3.249999999999999556, 12.18750000000000000, -2.153805922287440833 ) ) ;
#5804 = FACE_OUTER_BOUND ( 'NONE', #3983, .T. ) ;
#5805 = APPLICATION_CONTEXT ( 'configuration controlled 3d designs of mechanical parts and assemblies' ) ;
#5806 = CARTESIAN_POINT ( 'NONE',  ( -63.97645733981619998, 12.92636406023319395, -201.6791002821226755 ) ) ;
#5807 = ORIENTED_EDGE ( 'NONE', *, *, #9865, .T. ) ;
#5808 = EDGE_CURVE ( 'NONE', #14745, #745, #7839, .T. ) ;
#5809 = VERTEX_POINT ( 'NONE', #5591 ) ;
#5810 = DIRECTION ( 'NONE',  ( -0.000000000000000000, -1.000000000000000000, -0.000000000000000000 ) ) ;
#5811 = CARTESIAN_POINT ( 'NONE',  ( -1.553300858899106629, 5.062500000000001776, 0.2500000000000002220 ) ) ;
#5812 = CARTESIAN_POINT ( 'NONE',  ( -1.553300858899106629, 2.562500000000000444, 0.2499999999999998335 ) ) ;
#5813 = CARTESIAN_POINT ( 'NONE',  ( -9.000077715877306872, 2.500000000000000444, -105.4229635846035222 ) ) ;
#5814 = ORIENTED_EDGE ( 'NONE', *, *, #733, .T. ) ;
#5815 = CARTESIAN_POINT ( 'NONE',  ( 2.298097038856279362, 13.87500000000000000, -1.201902961143720860 ) ) ;
#5816 = CARTESIAN_POINT ( 'NONE',  ( -48.64052432076086063, 9.999999999999998224, -142.5706416652736266 ) ) ;
#5817 = CARTESIAN_POINT ( 'NONE',  ( -9.285933602755209293, 10.36776190932097386, -105.1819416493744654 ) ) ;
#5818 = CARTESIAN_POINT ( 'NONE',  ( -3.249999999999999556, 5.187500000000001776, -2.153805922287440833 ) ) ;
#5819 = CARTESIAN_POINT ( 'NONE',  ( 11.13433036043491242, 12.49999999999999822, -107.0267359326556829 ) ) ;
#5820 = CARTESIAN_POINT ( 'NONE',  ( 5.178267505235062629, 8.673617379884035472E-16, -121.9231527573877258 ) ) ;
#5821 = EDGE_LOOP ( 'NONE', ( #9041, #8238, #7353, #12397 ) ) ;
#5822 = DIRECTION ( 'NONE',  ( -0.8645818496218656835, 0.000000000000000000, 0.5024920151648518685 ) ) ;
#5823 = CARTESIAN_POINT ( 'NONE',  ( -3.980102097228897245E-16, 10.50000000000000000, -6.749999999999999112 ) ) ;
#5824 = ORIENTED_EDGE ( 'NONE', *, *, #2595, .T. ) ;
#5825 = ADVANCED_FACE ( 'NONE', ( #1967 ), #10013, .F. ) ;
#5826 = VERTEX_POINT ( 'NONE', #10306 ) ;
#5827 = DIRECTION ( 'NONE',  ( 1.770125995894655399E-15, 0.000000000000000000, -1.000000000000000000 ) ) ;
#5828 = CARTESIAN_POINT ( 'NONE',  ( -1.553300858899106629, 7.562500000000000888, 0.2500000000000002220 ) ) ;
#5829 = EDGE_CURVE ( 'NONE', #9311, #9630, #4099, .T. ) ;
#5830 = CARTESIAN_POINT ( 'NONE',  ( -3.980102097228897738E-16, 5.000000000000000000, -6.749999999999999112 ) ) ;
#5832 = EDGE_CURVE ( 'NONE', #12909, #814, #2246, .T. ) ;
#5831 = ORIENTED_EDGE ( 'NONE', *, *, #11568, .T. ) ;
#5833 = CARTESIAN_POINT ( 'NONE',  ( -3.249999999999999556, 4.187500000000000000, -2.153805922287440833 ) ) ;
#5834 = PRODUCT ( 'Washer_Predeterminado', 'Washer_Predeterminado', '', ( #10492 ) ) ;
#5835 = CARTESIAN_POINT ( 'NONE',  ( -3.749999999999999556, 10.31250000000000000, -5.053300858899104853 ) ) ;
#5836 = CARTESIAN_POINT ( 'NONE',  ( -25.42793803927663987, 0.04176024464420144411, -200.8198567788932110 ) ) ;
#5837 = CARTESIAN_POINT ( 'NONE',  ( 1.500000000000000000, 5.000000000000000000, 0.2500000000000002220 ) ) ;
#5838 = CARTESIAN_POINT ( 'NONE',  ( -6.683304552674626642, 0.000000000000000000, -104.1296019027811894 ) ) ;
#5839 = COORDINATED_UNIVERSAL_TIME_OFFSET ( 0, 0, .AHEAD. ) ;
#5840 = LINE ( 'NONE', #9402, #10240 ) ;
#5841 = AXIS2_PLACEMENT_3D ( 'NONE', #875, #7970, #2335 ) ;
#5842 = EDGE_LOOP ( 'NONE', ( #9955, #1557, #5341, #13453, #9405, #3366, #4045, #5695, #11013 ) ) ;
#5843 = CARTESIAN_POINT ( 'NONE',  ( 2.298097038856279362, 5.375000000000000000, -1.201902961143720860 ) ) ;
#5844 = CARTESIAN_POINT ( 'NONE',  ( -9.836272398077417378, 1.921202954650395700, -34.71741284551207229 ) ) ;
#5845 = CARTESIAN_POINT ( 'NONE',  ( 0.000000000000000000, 10.50000000000000000, 0.2499999999999998057 ) ) ;
#5846 = CARTESIAN_POINT ( 'NONE',  ( 1.114947364559091714, 4.793811891163896277, -139.4079432275550801 ) ) ;
#5847 = CARTESIAN_POINT ( 'NONE',  ( -67.63177441509803600, 12.98106818090269776, -202.0046632239205451 ) ) ;
#5848 = DIRECTION ( 'NONE',  ( -0.000000000000000000, -1.000000000000000000, -0.000000000000000000 ) ) ;
#5849 = CARTESIAN_POINT ( 'NONE',  ( -2.651650429449552870, 12.62500000000000000, -0.8483495705504463524 ) ) ;
#5850 = LINE ( 'NONE', #4701, #11690 ) ;
#5851 = PERSON_AND_ORGANIZATION ( #3176, #3020 ) ;
#5852 = CARTESIAN_POINT ( 'NONE',  ( 6.049910241306248437, 15.00000000000000000, -118.3734240199295300 ) ) ;
#5853 = CARTESIAN_POINT ( 'NONE',  ( -63.21422130130007133, 5.000000000000000000, -203.6040552426024703 ) ) ;
#5854 = ORIENTED_EDGE ( 'NONE', *, *, #14897, .F. ) ;
#5855 = CARTESIAN_POINT ( 'NONE',  ( -25.04988596881782570, 8.673617379884035472E-16, -199.3167991962343706 ) ) ;
#5856 = CARTESIAN_POINT ( 'NONE',  ( 3.249999999999999112, 2.812500000000000000, -2.153805922287439945 ) ) ;
#5857 = CARTESIAN_POINT ( 'NONE',  ( -60.56192452146473215, 15.00000000000000000, -187.5450233986829289 ) ) ;
#5858 = CARTESIAN_POINT ( 'NONE',  ( -3.980102097228897738E-16, 8.000000000000000000, -6.749999999999999112 ) ) ;
#5859 = ORIENTED_EDGE ( 'NONE', *, *, #10082, .F. ) ;
#5860 = CARTESIAN_POINT ( 'NONE',  ( -5.541218901316622869, 9.999999999999998224, -110.3933575420723372 ) ) ;
#5861 = CARTESIAN_POINT ( 'NONE',  ( 0.8629277978856378928, 12.44510974438689210, 2.552542045932815640 ) ) ;
#5862 = CARTESIAN_POINT ( 'NONE',  ( 8.054779650680396585, 15.00000000000000000, -130.1950568140550502 ) ) ;
#5863 = CARTESIAN_POINT ( 'NONE',  ( 1.346194077712558057, 1.562500000000000000, -6.750000000000000000 ) ) ;
#5864 = CARTESIAN_POINT ( 'NONE',  ( 0.000000000000000000, 11.50000000000000000, -0.2500000000000002220 ) ) ;
#5865 = CARTESIAN_POINT ( 'NONE',  ( 11.32016196459912649, 15.00000000000000000, -106.4092894470390291 ) ) ;
#5866 = CARTESIAN_POINT ( 'NONE',  ( 2.651650429449552870, 3.125000000000000444, -6.151650429449555091 ) ) ;
#5867 = CARTESIAN_POINT ( 'NONE',  ( 2.850044070969222521, 5.000000000000000888, -103.0233998225063345 ) ) ;
#5868 = DIRECTION ( 'NONE',  ( 0.9652928478129130241, 2.009419397152280694E-15, -0.2611699024796625968 ) ) ;
#5869 = CARTESIAN_POINT ( 'NONE',  ( 8.935548306746156300, 9.999999999999998224, 2.855381328098127725 ) ) ;
#5870 = CARTESIAN_POINT ( 'NONE',  ( 19.27433926169634049, 2.100000000000811884, 66.63156944101105239 ) ) ;
#5871 = CARTESIAN_POINT ( 'NONE',  ( 3.249999999999999556, 11.75000000000000000, -3.500000000000000000 ) ) ;
#5872 = PLANE ( 'NONE',  #13608 ) ;
#5873 = CARTESIAN_POINT ( 'NONE',  ( 5.079523875978591896, -9.029077709185064432E-12, -108.2552591983019994 ) ) ;
#5874 = EDGE_LOOP ( 'NONE', ( #6292, #13971, #12630, #3232 ) ) ;
#5875 = ORIENTED_EDGE ( 'NONE', *, *, #728, .T. ) ;
#5876 = CARTESIAN_POINT ( 'NONE',  ( -2.651064740270022035, 0.000000000000000000, -112.3760762047032387 ) ) ;
#5877 = CARTESIAN_POINT ( 'NONE',  ( 10.43870542337790930, 12.49999999999999822, -107.8020611273035883 ) ) ;
#5878 = CARTESIAN_POINT ( 'NONE',  ( -4.592425496802573972E-16, 6.500000000000000888, -7.249999999999999112 ) ) ;
#5879 = CARTESIAN_POINT ( 'NONE',  ( -2.651650429449552870, 3.875000000000000444, -6.151650429449552426 ) ) ;
#5880 = DIRECTION ( 'NONE',  ( 0.000000000000000000, 0.000000000000000000, 1.000000000000000000 ) ) ;
#5881 = ORIENTED_EDGE ( 'NONE', *, *, #532, .F. ) ;
#5882 = CARTESIAN_POINT ( 'NONE',  ( -4.873637833199961911, 1.564568837530078786E-16, -117.2491930705948988 ) ) ;
#5883 = CARTESIAN_POINT ( 'NONE',  ( 2.298097038856279362, 2.375000000000000000, -1.201902961143720860 ) ) ;
#5884 = CARTESIAN_POINT ( 'NONE',  ( -44.21823081166475333, 15.00000000000000000, -145.3603131190974125 ) ) ;
#5885 = CYLINDRICAL_SURFACE ( 'NONE', #8387, 2.000000000000001776 ) ;
#5886 = ADVANCED_FACE ( 'NONE', ( #4740 ), #9454, .T. ) ;
#5887 = CARTESIAN_POINT ( 'NONE',  ( -3.980102097228897245E-16, 5.500000000000000000, -6.749999999999999112 ) ) ;
#5888 = CALENDAR_DATE ( 2026, 8, 10 ) ;
#5889 = DIRECTION ( 'NONE',  ( 0.000000000000000000, 0.000000000000000000, -1.000000000000000000 ) ) ;
#5890 = CARTESIAN_POINT ( 'NONE',  ( 22.59539982210069553, 8.673617379884035472E-16, -140.1889075229756259 ) ) ;
#5891 = VERTEX_POINT ( 'NONE', #8285 ) ;
#5892 = CARTESIAN_POINT ( 'NONE',  ( -0.2180828300734916347, 15.00000000000000178, -115.1409152625263346 ) ) ;
#5893 = DIRECTION ( 'NONE',  ( -0.000000000000000000, -1.000000000000000000, -0.000000000000000000 ) ) ;
#5894 = ORIENTED_EDGE ( 'NONE', *, *, #8014, .T. ) ;
#5895 = ORIENTED_EDGE ( 'NONE', *, *, #368, .T. ) ;
#5896 = CARTESIAN_POINT ( 'NONE',  ( -0.3766621274091715987, 0.5000000000000000000, -0.1347136637304948981 ) ) ;
#5897 = CARTESIAN_POINT ( 'NONE',  ( 3.749999999999999112, 5.187500000000001776, -5.053300858899108405 ) ) ;
#5898 = CARTESIAN_POINT ( 'NONE',  ( -3.249999999999999556, 5.750000000000000888, -3.500000000000000000 ) ) ;
#5899 = EDGE_LOOP ( 'NONE', ( #3678, #15281, #369, #9461 ) ) ;
#5900 = CARTESIAN_POINT ( 'NONE',  ( 6.256842659011002006, 14.34211104607853393, 2.774933013893350786 ) ) ;
#5901 = CARTESIAN_POINT ( 'NONE',  ( -3.249999999999999556, 1.250000000000000000, -3.499999999999999556 ) ) ;
#5902 = CC_DESIGN_SECURITY_CLASSIFICATION ( #7881, ( #15317 ) ) ;
#5903 = AXIS2_PLACEMENT_3D ( 'NONE', #3718, #4730, #14240 ) ;
#5904 = B_SPLINE_CURVE_WITH_KNOTS ( 'NONE', 3,
 ( #4874, #14640, #4037, #4952, #167, #9586, #9826, #1705, #6189, #6271, #3717, #7421, #14312, #3879, #10750, #8742, #7266, #1401, #10986, #8422, #10904, #13474 ),
 .UNSPECIFIED., .F., .F.,
 ( 4, 2, 2, 2, 2, 2, 2, 2, 2, 2, 4 ),
 ( 8.673617379884035472E-19, 0.001106625736872399440, 0.002213251473744798012, 0.002766564342180997081, 0.003319877210617196584, 0.004426502947489592554, 0.005533128684361988958, 0.006639754421234385362, 0.007746380158106782633, 0.008299693026542979968, 0.008853005894979178170 ),
 .UNSPECIFIED. ) ;
#5905 = CARTESIAN_POINT ( 'NONE',  ( -7.398315985760856250, 9.999999999999998224, -123.5712579988217072 ) ) ;
#5906 = ADVANCED_FACE ( 'NONE', ( #2349, #4592 ), #1036, .F. ) ;
#5907 = CARTESIAN_POINT ( 'NONE',  ( -16.94138229547582242, 9.999999999999998224, -154.2864167784019003 ) ) ;
#5908 = EDGE_CURVE ( 'NONE', #6054, #7799, #6847, .T. ) ;
#5909 = CARTESIAN_POINT ( 'NONE',  ( 7.148068729939690336, -2.490287375297125294, -34.56909192082981974 ) ) ;
#5910 = APPROVAL_STATUS ( 'not_yet_approved' ) ;
#5911 = CARTESIAN_POINT ( 'NONE',  ( 2.920755695452265766, 1.195290186917868480, -1.000000000000001110 ) ) ;
#5912 = CC_DESIGN_SECURITY_CLASSIFICATION ( #12585, ( #15323 ) ) ;
#5913 = VERTEX_POINT ( 'NONE', #6826 ) ;
#5914 = TOROIDAL_SURFACE ( 'NONE', #11603, 5.000000000000001776, 5.000000000000000000 ) ;
#5915 = CARTESIAN_POINT ( 'NONE',  ( -9.742503157198443731, 2.490287375297125294, -40.35209559314896666 ) ) ;
#5916 = CARTESIAN_POINT ( 'NONE',  ( -3.749999999999999556, 12.75000000000000178, -3.499999999999999112 ) ) ;
#5917 = CYLINDRICAL_SURFACE ( 'NONE', #278, 3.500000000000000000 ) ;
#5918 = VECTOR ( 'NONE', #14736, 1000.000000000000000 ) ;
#5919 = CARTESIAN_POINT ( 'NONE',  ( -67.60945598279326418, 13.34030093848967269, -201.1617207694782223 ) ) ;
#5920 = DIRECTION ( 'NONE',  ( 0.000000000000000000, 1.000000000000000000, 0.000000000000000000 ) ) ;
#5921 = CARTESIAN_POINT ( 'NONE',  ( 1.346194077712558279, 3.062500000000000000, -6.750000000000000888 ) ) ;
#5922 = CARTESIAN_POINT ( 'NONE',  ( 9.508011421805740326, 1.297355693583747804, -106.3802021279168031 ) ) ;
#5923 = AXIS2_PLACEMENT_3D ( 'NONE', #10643, #13508, #5996 ) ;
#5924 = ADVANCED_FACE ( 'NONE', ( #5662 ), #3584, .T. ) ;
#5925 = DATE_TIME_ROLE ( 'classification_date' ) ;
#5926 = CIRCLE ( 'NONE', #3223, 5.000000000000000000 ) ;
#5927 = CARTESIAN_POINT ( 'NONE',  ( -15.73004658022870927, 0.000000000000000000, -131.7446186346720367 ) ) ;
#5928 = ORIENTED_EDGE ( 'NONE', *, *, #14445, .T. ) ;
#5929 = CARTESIAN_POINT ( 'NONE',  ( 7.906415743051303124, 1.937363517912831012, 2.211849553340444530 ) ) ;
#5930 = CARTESIAN_POINT ( 'NONE',  ( -3.249999999999999556, 2.187500000000000444, -2.153805922287440833 ) ) ;
#5931 = B_SPLINE_CURVE_WITH_KNOTS ( 'NONE', 3,
 ( #3141, #12573, #6704, #15290, #6780, #7067, #4543, #3216, #4461, #2295, #12885, #4759, #14125, #9398 ),
 .UNSPECIFIED., .F., .F.,
 ( 4, 2, 2, 2, 2, 2, 4 ),
 ( 0.000000000000000000, 0.004869271879394969707, 0.007303907819092454561, 0.009738543758789939414, 0.01460781563818490912, 0.01704245157788239484, 0.01947708751757987883 ),
 .UNSPECIFIED. ) ;
#5932 = CARTESIAN_POINT ( 'NONE',  ( -61.08087366679612984, 15.00000000000267164, -189.6635742862125085 ) ) ;
#5933 = CIRCLE ( 'NONE', #15091, 3.000000000000010214 ) ;
#5934 = CARTESIAN_POINT ( 'NONE',  ( 1.346194077712561166, 6.437500000000000888, -0.2500000000000011102 ) ) ;
#5935 = EDGE_LOOP ( 'NONE', ( #12672, #4095, #12699, #12643 ) ) ;
#5936 = CARTESIAN_POINT ( 'NONE',  ( -5.254015288333886424, 9.999999999999998224, -115.0648584343545764 ) ) ;
#5937 = CONICAL_SURFACE ( 'NONE', #3992, 0.4999999999999865663, 0.6283185307179600665 ) ;
#5938 = CARTESIAN_POINT ( 'NONE',  ( 3.892182721467340123, 14.89914772901184747, -1.394991539848200457 ) ) ;
#5939 = CARTESIAN_POINT ( 'NONE',  ( -16.94138229547579400, 9.999999999999998224, -154.2864167784019287 ) ) ;
#5940 = CARTESIAN_POINT ( 'NONE',  ( -3.249999999999999556, 1.312500000000000444, -4.846194077712557835 ) ) ;
#5941 = CARTESIAN_POINT ( 'NONE',  ( -1.346194077712559167, 14.93750000000000000, -6.749999999999999112 ) ) ;
#5942 = CARTESIAN_POINT ( 'NONE',  ( -3.750000000000000000, 7.250000000000000000, -3.499999999999999112 ) ) ;
#5943 = CARTESIAN_POINT ( 'NONE',  ( 0.2116200952963268878, 8.673617379884035472E-16, -112.6243614187691975 ) ) ;
#5944 = CARTESIAN_POINT ( 'NONE',  ( 3.749999999999999112, 4.187500000000000888, -5.053300858899108405 ) ) ;
#5945 = CARTESIAN_POINT ( 'NONE',  ( 3.189625183574164247, 14.71804858691771578, 2.256190190007254515 ) ) ;
#5946 = CIRCLE ( 'NONE', #7933, 3.000000000000000000 ) ;
#5947 = CARTESIAN_POINT ( 'NONE',  ( -8.886921396801742645, 9.999999999999998224, -105.5168766094550676 ) ) ;
#5948 = CARTESIAN_POINT ( 'NONE',  ( 7.148068729939690336, -2.490287375297125294, -34.56909192082981974 ) ) ;
#5949 = CARTESIAN_POINT ( 'NONE',  ( 3.230086961373092702, 10.41478694124928239, 5.208283729180116062 ) ) ;
#5950 = CARTESIAN_POINT ( 'NONE',  ( 1.346194077712558057, 12.56250000000000000, -6.750000000000000000 ) ) ;
#5951 = CARTESIAN_POINT ( 'NONE',  ( -8.754992051701663058, 12.12271237224970477, -104.5108651954749917 ) ) ;
#5952 = CARTESIAN_POINT ( 'NONE',  ( -63.47082007717695973, 11.73238145425375301, -203.0222944482916887 ) ) ;
#5953 = ORIENTED_EDGE ( 'NONE', *, *, #224, .T. ) ;
#5954 = PRODUCT_DEFINITION_SHAPE ( 'NONE', 'NONE',  #15322 ) ;
#5955 = ORIENTED_EDGE ( 'NONE', *, *, #648, .T. ) ;
#5956 = CARTESIAN_POINT ( 'NONE',  ( -5.137754182365905642, -1.054997312397557146E-12, -114.0283549521487174 ) ) ;
#5957 = CARTESIAN_POINT ( 'NONE',  ( 9.010117806275914631, 12.49999999999999822, -110.1316647874338202 ) ) ;
#5958 = CARTESIAN_POINT ( 'NONE',  ( -2.651650429449552870, 6.125000000000000000, -0.8483495705504462414 ) ) ;
#5959 = CARTESIAN_POINT ( 'NONE',  ( 1.553300858899105963, 6.062500000000000000, -7.249999999999999112 ) ) ;
#5960 = CARTESIAN_POINT ( 'NONE',  ( -1.500000000000000000, 4.500000000000000888, -0.2499999999999997780 ) ) ;
#5961 = VERTEX_POINT ( 'NONE', #13779 ) ;
#5962 = CIRCLE ( 'NONE', #13120, 1.000000000000000888 ) ;
#5963 = CARTESIAN_POINT ( 'NONE',  ( -4.234402844927157794, 4.336808689942017736E-16, -117.4888040839639558 ) ) ;
#5964 = CARTESIAN_POINT ( 'NONE',  ( 1.346194077712561166, 1.437500000000000000, -0.2500000000000011102 ) ) ;
#5965 = CARTESIAN_POINT ( 'NONE',  ( -0.4873557683217199510, 5.000000000000001776, -103.5659326153046038 ) ) ;
#5966 = CARTESIAN_POINT ( 'NONE',  ( 0.000000000000000000, 0.2006112523677016646, 0.1491815183709511716 ) ) ;
#5967 =( NAMED_UNIT ( * ) PLANE_ANGLE_UNIT ( ) SI_UNIT ( $, .RADIAN. ) );
#5968 = CARTESIAN_POINT ( 'NONE',  ( 1.346194077712560944, 3.937500000000000000, -0.2500000000000010547 ) ) ;
#5969 = AXIS2_PLACEMENT_3D ( 'NONE', #9456, #7359, #8520 ) ;
#5970 = CARTESIAN_POINT ( 'NONE',  ( 7.965741386218653020, 15.00000000000000000, -106.9514265361661387 ) ) ;
#5971 = CARTESIAN_POINT ( 'NONE',  ( 15.55587903137338834, -8.452217897303065567E-13, -128.0070267004813900 ) ) ;
#5972 = EDGE_LOOP ( 'NONE', ( #10754, #14567, #8034, #13582, #7710, #2428 ) ) ;
#5973 = CARTESIAN_POINT ( 'NONE',  ( -1.065067592858583323, 15.00000000000000178, -118.9225514786646016 ) ) ;
#5974 = CARTESIAN_POINT ( 'NONE',  ( -3.249999999999999556, 13.31250000000000000, -4.846194077712557835 ) ) ;
#5975 = ORIENTED_EDGE ( 'NONE', *, *, #13596, .F. ) ;
#5976 = ORIENTED_EDGE ( 'NONE', *, *, #1166, .T. ) ;
#5977 = CYLINDRICAL_SURFACE ( 'NONE', #12936, 1.000000000000000888 ) ;
#5978 = CARTESIAN_POINT ( 'NONE',  ( -4.592425496802573972E-16, 4.000000000000000888, -7.250000000000000000 ) ) ;
#5979 = CARTESIAN_POINT ( 'NONE',  ( -3.980102097228897738E-16, 10.00000000000000000, -6.749999999999999112 ) ) ;
#5980 = ORIENTED_EDGE ( 'NONE', *, *, #14788, .T. ) ;
#5981 = EDGE_CURVE ( 'NONE', #2589, #8920, #7889, .T. ) ;
#5982 = CARTESIAN_POINT ( 'NONE',  ( 6.347577276663199264, 14.84036095819059220, 1.566136529894637253 ) ) ;
#5983 = CARTESIAN_POINT ( 'NONE',  ( -3.249999999999999556, 4.312500000000000888, -4.846194077712557835 ) ) ;
#5984 = CARTESIAN_POINT ( 'NONE',  ( -9.153863602783623321, 1.835169552024503936, -104.6442049519377804 ) ) ;
#5985 = CARTESIAN_POINT ( 'NONE',  ( -52.54183813970617223, 9.999999999999996447, -168.5664894671085392 ) ) ;
#5986 = AXIS2_PLACEMENT_3D ( 'NONE', #12743, #14995, #5476 ) ;
#5987 = CARTESIAN_POINT ( 'NONE',  ( 7.125599087756446792, 15.00000000000000000, -120.1321298350141831 ) ) ;
#5988 = PERSON_AND_ORGANIZATION ( #3176, #3020 ) ;
#5989 = DIRECTION ( 'NONE',  ( -0.02181900108494732801, 0.000000000000000000, 0.9997619372588931741 ) ) ;
#5990 = VERTEX_POINT ( 'NONE', #6587 ) ;
#5991 = ADVANCED_FACE ( 'NONE', ( #14879 ), #11298, .T. ) ;
#5992 = FACE_OUTER_BOUND ( 'NONE', #10473, .T. ) ;
#5993 = EDGE_CURVE ( 'NONE', #11845, #11885, #8828, .T. ) ;
#5994 = VECTOR ( 'NONE', #13468, 1000.000000000000114 ) ;
#5995 = CARTESIAN_POINT ( 'NONE',  ( 2.651650429449552870, 14.12500000000000000, -6.151650429449553314 ) ) ;
#5996 = DIRECTION ( 'NONE',  ( 0.000000000000000000, 0.000000000000000000, 1.000000000000000000 ) ) ;
#5997 = CARTESIAN_POINT ( 'NONE',  ( -67.58823768853794434, 10.57596889791075867, -204.4395760673659197 ) ) ;
#5998 = CARTESIAN_POINT ( 'NONE',  ( 0.000000000000000000, 3.500000000000000000, -0.2500000000000002220 ) ) ;
#5999 = CARTESIAN_POINT ( 'NONE',  ( 10.58852313474634421, 2.370005426030849627, -106.5284185414804199 ) ) ;
#6000 = MECHANICAL_CONTEXT ( 'NONE', #10340, 'mechanical' ) ;
#6001 = DIRECTION ( 'NONE',  ( 0.000000000000000000, 1.000000000000000000, 0.000000000000000000 ) ) ;
#6002 = CIRCLE ( 'NONE', #11698, 1.000000000000000888 ) ;
#6003 = CARTESIAN_POINT ( 'NONE',  ( 0.3766621274091715987, 0.5000000000000000000, -7.146945437571387671 ) ) ;
#6004 = AXIS2_PLACEMENT_3D ( 'NONE', #14948, #1709, #6654 ) ;
#6005 = VERTEX_POINT ( 'NONE', #4350 ) ;
#6006 = CARTESIAN_POINT ( 'NONE',  ( 4.033098156701212744, 0.09438068890001453937, -1.663700395152667211 ) ) ;
#6007 = CARTESIAN_POINT ( 'NONE',  ( 3.249999999999999556, 3.750000000000000000, -3.500000000000000000 ) ) ;
#6008 = CARTESIAN_POINT ( 'NONE',  ( -47.48189921986828210, 9.999999999999998224, -141.5723758807981483 ) ) ;
#6009 = EDGE_CURVE ( 'NONE', #12700, #9908, #8757, .T. ) ;
#6010 = CARTESIAN_POINT ( 'NONE',  ( -3.249999999999999112, 7.687500000000000888, -2.153805922287440833 ) ) ;
#6011 = EDGE_LOOP ( 'NONE', ( #9590, #14430, #44, #11252 ) ) ;
#6012 = CARTESIAN_POINT ( 'NONE',  ( -0.5690871621892230614, 14.99999999999999822, -109.6097011989409111 ) ) ;
#6013 = EDGE_CURVE ( 'NONE', #119, #10778, #15309, .T. ) ;
#6014 = DIRECTION ( 'NONE',  ( 0.000000000000000000, 1.000000000000000000, 0.000000000000000000 ) ) ;
#6015 = ADVANCED_FACE ( 'NONE', ( #646 ), #13488, .F. ) ;
#6016 = CYLINDRICAL_SURFACE ( 'NONE', #12934, 6.999999999999950262 ) ;
#6017 = CARTESIAN_POINT ( 'NONE',  ( -1.346194077712559389, 2.437500000000000444, -6.749999999999999112 ) ) ;
#6018 = AXIS2_PLACEMENT_3D ( 'NONE', #1599, #13352, #6382 ) ;
#6019 = CARTESIAN_POINT ( 'NONE',  ( -2.651650429449552870, 2.875000000000000000, -6.151650429449552426 ) ) ;
#6020 = CARTESIAN_POINT ( 'NONE',  ( 1.553300858899108849, 5.937500000000000000, 0.2499999999999993616 ) ) ;
#6021 = CARTESIAN_POINT ( 'NONE',  ( 0.000000000000000000, 1.000000000000000000, -6.000000000000002665 ) ) ;
#6022 = CARTESIAN_POINT ( 'NONE',  ( 1.553300858899105963, 8.062500000000001776, -7.250000000000000888 ) ) ;
#6023 = CARTESIAN_POINT ( 'NONE',  ( 3.489143780149524421, 14.82608718968779371, 1.723058558630278014 ) ) ;
#6024 = DIRECTION ( 'NONE',  ( 2.672056983927306126E-18, 1.000000000000000000, -1.224355256373460583E-16 ) ) ;
#6025 = LINE ( 'NONE', #5033, #2442 ) ;
#6026 = CARTESIAN_POINT ( 'NONE',  ( 1.078231930479242484, 5.000000000000000888, -139.4303258909232852 ) ) ;
#6027 = CARTESIAN_POINT ( 'NONE',  ( 1.346194077712560944, 13.93750000000000000, -0.2500000000000010547 ) ) ;
#6028 = AXIS2_PLACEMENT_3D ( 'NONE', #9438, #1169, #8 ) ;
#6029 = CARTESIAN_POINT ( 'NONE',  ( -8.422539546171003977, 12.70549722942692661, -104.4083970429161639 ) ) ;
#6030 = FACE_OUTER_BOUND ( 'NONE', #10084, .T. ) ;
#6031 = AXIS2_PLACEMENT_3D ( 'NONE', #14050, #12577, #9330 ) ;
#6032 = ORIENTED_EDGE ( 'NONE', *, *, #14541, .T. ) ;
#6033 = CARTESIAN_POINT ( 'NONE',  ( -3.750000000000000000, 8.812500000000001776, -5.053300858899105741 ) ) ;
#6034 = VERTEX_POINT ( 'NONE', #5352 ) ;
#6035 = CARTESIAN_POINT ( 'NONE',  ( -6.701857729235380923, -1.323436422439033798E-13, -119.5348842628491042 ) ) ;
#6036 = CARTESIAN_POINT ( 'NONE',  ( 8.475206276408092876, 0.000000000000000000, -34.56909192082981974 ) ) ;
#6037 = CARTESIAN_POINT ( 'NONE',  ( 3.750000000000000000, 5.750000000000000000, -3.500000000000000444 ) ) ;
#6038 = CARTESIAN_POINT ( 'NONE',  ( -1.553300858899107073, 4.937500000000000000, -7.249999999999999112 ) ) ;
#6039 = CARTESIAN_POINT ( 'NONE',  ( -0.9087754948914270603, 0.000000000000000000, -36.05536862169275025 ) ) ;
#6040 = ORIENTED_EDGE ( 'NONE', *, *, #12736, .F. ) ;
#6041 = VECTOR ( 'NONE', #11729, 1000.000000000000000 ) ;
#6042 = CARTESIAN_POINT ( 'NONE',  ( 3.249999999999999556, 6.250000000000000000, -3.500000000000000000 ) ) ;
#6043 = CC_DESIGN_PERSON_AND_ORGANIZATION_ASSIGNMENT ( #8250, #9267, ( #9258 ) ) ;
#6044 = CARTESIAN_POINT ( 'NONE',  ( -60.12955526703344589, 15.00000000000000000, -169.2020697305022736 ) ) ;
#6045 = DIRECTION ( 'NONE',  ( 0.06144244613646117348, 0.7154473348115029108, 0.6959597236362787820 ) ) ;
#6046 = CARTESIAN_POINT ( 'NONE',  ( 1.346194077712558057, 9.562500000000000000, -6.750000000000000000 ) ) ;
#6047 = CARTESIAN_POINT ( 'NONE',  ( -9.492276966213163192, 10.00000000001546674, -117.3221826544872215 ) ) ;
#6048 = COORDINATED_UNIVERSAL_TIME_OFFSET ( 0, 0, .AHEAD. ) ;
#6049 = CARTESIAN_POINT ( 'NONE',  ( 4.544676675852343806, 15.00000000000000000, -126.1782412829290934 ) ) ;
#6050 = CARTESIAN_POINT ( 'NONE',  ( 23.85593715798673031, 8.673617379884035472E-16, -134.9913929664622287 ) ) ;
#6051 = ORIENTED_EDGE ( 'NONE', *, *, #12707, .F. ) ;
#6052 = FACE_OUTER_BOUND ( 'NONE', #143, .T. ) ;
#6053 = CARTESIAN_POINT ( 'NONE',  ( 3.249999999999999112, 13.81250000000000000, -2.153805922287439945 ) ) ;
#6054 = VERTEX_POINT ( 'NONE', #10067 ) ;
#6055 = ORIENTED_EDGE ( 'NONE', *, *, #7781, .T. ) ;
#6056 = CARTESIAN_POINT ( 'NONE',  ( -0.2511109529196363654, 0.2068841402060896395, 0.1491815183709511161 ) ) ;
#6057 =( BOUNDED_CURVE ( )  B_SPLINE_CURVE ( 3, ( #6510, #2101, #11225, #6735 ),
 .UNSPECIFIED., .F., .T. ) 
 B_SPLINE_CURVE_WITH_KNOTS ( ( 4, 4 ),
 ( 0.2828104278872010102, 0.5984188431165737843 ),
 .UNSPECIFIED. ) 
 CURVE ( )  GEOMETRIC_REPRESENTATION_ITEM ( )  RATIONAL_B_SPLINE_CURVE ( ( 1.000000000000000000, 0.9917164885600966429, 0.9917164885600966429, 1.000000000000000000 ) ) 
 REPRESENTATION_ITEM ( '' )  );
#6058 = CARTESIAN_POINT ( 'NONE',  ( -4.592425496802573972E-16, 7.000000000000000000, -7.250000000000000000 ) ) ;
#6059 = CARTESIAN_POINT ( 'NONE',  ( 1.346194077712561166, 12.43750000000000000, -0.2500000000000011102 ) ) ;
#6060 = VERTEX_POINT ( 'NONE', #2027 ) ;
#6061 = CARTESIAN_POINT ( 'NONE',  ( 6.122889832264990950, 10.33058039608724954, 5.281130614573721793 ) ) ;
#6062 = CARTESIAN_POINT ( 'NONE',  ( -3.980102097228897245E-16, 5.500000000000000000, -6.749999999999999112 ) ) ;
#6063 = CARTESIAN_POINT ( 'NONE',  ( -4.492499072540820926, 0.000000000000000000, 2.611025101989610686 ) ) ;
#6064 = CARTESIAN_POINT ( 'NONE',  ( -61.15244389481968312, 10.00000000000000000, -189.9478847066162643 ) ) ;
#6065 = EDGE_CURVE ( 'NONE', #14402, #9864, #527, .T. ) ;
#6066 = CARTESIAN_POINT ( 'NONE',  ( -62.93226630389403908, 14.99999999999999822, -178.2952964610624349 ) ) ;
#6067 = MECHANICAL_CONTEXT ( 'NONE', #2448, 'mechanical' ) ;
#6068 = CARTESIAN_POINT ( 'NONE',  ( 0.2499999999999999445, 4.500000000000000888, 0.2500000000000002220 ) ) ;
#6069 = ORIENTED_EDGE ( 'NONE', *, *, #10183, .T. ) ;
#6070 = CARTESIAN_POINT ( 'NONE',  ( 2.298097038856278473, 9.625000000000000000, -5.798097038856279362 ) ) ;
#6071 = CARTESIAN_POINT ( 'NONE',  ( 2.298097038856279362, 13.37500000000000000, -1.201902961143720860 ) ) ;
#6072 = B_SPLINE_CURVE_WITH_KNOTS ( 'NONE', 3,
 ( #10435, #1085, #11442, #4489 ),
 .UNSPECIFIED., .F., .F.,
 ( 4, 4 ),
 ( 0.000000000000000000, 0.03035464128818402690 ),
 .UNSPECIFIED. ) ;
#6073 = CARTESIAN_POINT ( 'NONE',  ( -2.524281728693006599, 7.379999999999995453, -45.64919840677852392 ) ) ;
#6074 = CARTESIAN_POINT ( 'NONE',  ( -3.749999999999999556, 13.75000000000000000, -3.499999999999999112 ) ) ;
#6075 = CARTESIAN_POINT ( 'NONE',  ( -63.84839520601438778, 10.76401871533024313, -211.4757790814346947 ) ) ;
#6076 = DIRECTION ( 'NONE',  ( 0.000000000000000000, 0.000000000000000000, -1.000000000000000000 ) ) ;
#6077 = CARTESIAN_POINT ( 'NONE',  ( 3.249999999999999556, 4.250000000000000000, -3.500000000000000000 ) ) ;
#6078 = CARTESIAN_POINT ( 'NONE',  ( -8.661991262811106651, 15.00000000000000000, -130.6821289911104316 ) ) ;
#6079 = PERSON_AND_ORGANIZATION ( #3176, #3020 ) ;
#6080 = ADVANCED_FACE ( 'NONE', ( #2956 ), #6739, .T. ) ;
#6081 = CARTESIAN_POINT ( 'NONE',  ( -2.935443650368948276, 14.73055553252727634, -125.3529989061166532 ) ) ;
#6082 = LINE ( 'NONE', #4777, #11367 ) ;
#6083 = ORIENTED_EDGE ( 'NONE', *, *, #7993, .T. ) ;
#6084 = CARTESIAN_POINT ( 'NONE',  ( 4.892667292236299481, 0.02568563158750709549, 0.3754323223072091875 ) ) ;
#6085 = CARTESIAN_POINT ( 'NONE',  ( -1.346194077712558945, 8.062500000000000000, -0.2500000000000002220 ) ) ;
#6086 = CARTESIAN_POINT ( 'NONE',  ( -8.630633989116716975, 0.8298274931565884360, -104.9068229896404461 ) ) ;
#6087 = CARTESIAN_POINT ( 'NONE',  ( 0.000000000000000000, 12.00000000000000000, -0.2500000000000002220 ) ) ;
#6088 = CARTESIAN_POINT ( 'NONE',  ( -2.298097038856279362, 6.875000000000000000, -5.798097038856278473 ) ) ;
#6089 = CARTESIAN_POINT ( 'NONE',  ( -1.056049066447270590, 15.00000000000000000, -118.8733157714634672 ) ) ;
#6090 = AXIS2_PLACEMENT_3D ( 'NONE', #10924, #3898, #6209 ) ;
#6091 = CARTESIAN_POINT ( 'NONE',  ( -0.3766621274091715432, -0.2054769798019681903, -0.1347136637304948981 ) ) ;
#6092 = CARTESIAN_POINT ( 'NONE',  ( 10.01939027896081491, 15.00000000000000000, -127.6977514918621637 ) ) ;
#6093 = CC_DESIGN_PERSON_AND_ORGANIZATION_ASSIGNMENT ( #3919, #11026, ( #8846 ) ) ;
#6094 = CARTESIAN_POINT ( 'NONE',  ( 1.346194077712558057, 0.5625000000000001110, -6.750000000000000000 ) ) ;
#6095 = CARTESIAN_POINT ( 'NONE',  ( -2.651650429449552870, 1.625000000000000000, -0.8483495705504467965 ) ) ;
#6096 = CARTESIAN_POINT ( 'NONE',  ( -2.651650429449553314, 6.375000000000000888, -6.151650429449552426 ) ) ;
#6097 = CARTESIAN_POINT ( 'NONE',  ( -4.057877601665376588, 10.61085214779863151, -45.92595659261393592 ) ) ;
#6098 = CARTESIAN_POINT ( 'NONE',  ( 2.651650429449552870, 6.125000000000000000, -6.151650429449555091 ) ) ;
#6099 = CARTESIAN_POINT ( 'NONE',  ( 3.477102512744043583, 11.93308722758116147, 4.762272240101847132 ) ) ;
#6100 = DIRECTION ( 'NONE',  ( 0.000000000000000000, -1.000000000000000000, 0.000000000000000000 ) ) ;
#6101 = EDGE_CURVE ( 'NONE', #9696, #447, #7746, .T. ) ;
#6102 = EDGE_CURVE ( 'NONE', #13770, #3511, #5162, .T. ) ;
#6103 = CARTESIAN_POINT ( 'NONE',  ( -5.445322652854981627, 5.900679960901947346E-16, 1.000000000000000000 ) ) ;
#6104 = EDGE_CURVE ( 'NONE', #16, #4737, #1231, .T. ) ;
#6105 = CARTESIAN_POINT ( 'NONE',  ( 2.394576890926103818, 8.673617379884035472E-16, -144.4837070969091712 ) ) ;
#6106 = CARTESIAN_POINT ( 'NONE',  ( 3.249999999999999112, 10.81250000000000178, -2.153805922287439945 ) ) ;
#6107 = CARTESIAN_POINT ( 'NONE',  ( 2.538752285253552454, -6.419766481290676335E-32, -144.3958141051384985 ) ) ;
#6108 = CARTESIAN_POINT ( 'NONE',  ( -63.75486902486332497, 12.47328257159134779, -202.3017344482634030 ) ) ;
#6109 = ORIENTED_EDGE ( 'NONE', *, *, #367, .F. ) ;
#6110 = CC_DESIGN_PERSON_AND_ORGANIZATION_ASSIGNMENT ( #10272, #12383, ( #10417 ) ) ;
#6111 = CARTESIAN_POINT ( 'NONE',  ( -4.592425496802573972E-16, 8.999999999999998224, -7.250000000000000000 ) ) ;
#6112 = ORIENTED_EDGE ( 'NONE', *, *, #2154, .T. ) ;
#6113 = CARTESIAN_POINT ( 'NONE',  ( -6.399074640931504021, 2.500000000000000444, -108.4234853095435369 ) ) ;
#6114 = CARTESIAN_POINT ( 'NONE',  ( -24.29516989927810400, 3.999999999999602096, -208.1346784444976095 ) ) ;
#6115 = CARTESIAN_POINT ( 'NONE',  ( -1.553300858899107295, 7.437500000000000888, -7.250000000000000000 ) ) ;
#6116 = CARTESIAN_POINT ( 'NONE',  ( -3.750000000000000000, 4.687500000000000000, -1.946699141100893149 ) ) ;
#6117 = FACE_OUTER_BOUND ( 'NONE', #14781, .T. ) ;
#6118 = EDGE_LOOP ( 'NONE', ( #13586, #1104 ) ) ;
#6119 = CARTESIAN_POINT ( 'NONE',  ( -3.249999999999999556, 2.750000000000000444, -3.500000000000000000 ) ) ;
#6120 = B_SPLINE_CURVE_WITH_KNOTS ( 'NONE', 3,
 ( #10817, #10671, #13065, #10982, #8576, #9750 ),
 .UNSPECIFIED., .F., .F.,
 ( 4, 2, 4 ),
 ( 0.0002107453662977397553, 0.01553454269887521305, 0.03085834003145268567 ),
 .UNSPECIFIED. ) ;
#6121 = CARTESIAN_POINT ( 'NONE',  ( -3.749999999999999556, 8.312500000000000000, -5.053300858899104853 ) ) ;
#6122 = CARTESIAN_POINT ( 'NONE',  ( -64.62739667067044991, 15.00000000000000000, -185.6367153532767986 ) ) ;
#6123 = CARTESIAN_POINT ( 'NONE',  ( 3.704461453187086750, 8.673617379884037444E-16, -110.4530743311176479 ) ) ;
#6124 =( LENGTH_UNIT ( ) NAMED_UNIT ( * ) SI_UNIT ( .MILLI., .METRE. ) );
#6125 = CARTESIAN_POINT ( 'NONE',  ( -1.346194077712559389, 6.062500000000000000, -0.2500000000000002220 ) ) ;
#6126 = ADVANCED_FACE ( 'NONE', ( #3405 ), #5799, .T. ) ;
#6127 = DIRECTION ( 'NONE',  ( 0.000000000000000000, 1.000000000000000000, 0.000000000000000000 ) ) ;
#6128 = LINE ( 'NONE', #10843, #3818 ) ;
#6129 = CARTESIAN_POINT ( 'NONE',  ( 10.87631271617703987, 5.000000000000000888, -121.9832090783556140 ) ) ;
#6130 = CC_DESIGN_PERSON_AND_ORGANIZATION_ASSIGNMENT ( #11185, #10187, ( #5003 ) ) ;
#6131 = VERTEX_POINT ( 'NONE', #13935 ) ;
#6132 = DIRECTION ( 'NONE',  ( 0.000000000000000000, 0.000000000000000000, -1.000000000000000000 ) ) ;
#6133 = DIRECTION ( 'NONE',  ( 0.000000000000000000, 0.000000000000000000, -1.000000000000000000 ) ) ;
#6134 = VERTEX_POINT ( 'NONE', #14080 ) ;
#6135 = VERTEX_POINT ( 'NONE', #8114 ) ;
#6136 = LINE ( 'NONE', #6219, #11194 ) ;
#6137 = CARTESIAN_POINT ( 'NONE',  ( 2.651650429449553314, 14.37500000000000000, -0.8483495705504476847 ) ) ;
#6138 = CARTESIAN_POINT ( 'NONE',  ( -3.249999999999999556, 7.750000000000000888, -3.500000000000000000 ) ) ;
#6139 = CARTESIAN_POINT ( 'NONE',  ( -1.346194077712559167, 9.937500000000001776, -6.749999999999999112 ) ) ;
#6140 = ORIENTED_EDGE ( 'NONE', *, *, #3371, .F. ) ;
#6141 = CARTESIAN_POINT ( 'NONE',  ( -12.80600979999658762, 8.673617379884035472E-16, -182.2240817400024184 ) ) ;
#6142 = CARTESIAN_POINT ( 'NONE',  ( -2.298097038856278473, 7.125000000000000000, -1.201902961143720416 ) ) ;
#6143 = DIRECTION ( 'NONE',  ( -0.000000000000000000, -0.000000000000000000, 1.000000000000000000 ) ) ;
#6144 = DIRECTION ( 'NONE',  ( 0.9961255586397056438, 0.000000000000000000, -0.08794243244722427244 ) ) ;
#6145 = CARTESIAN_POINT ( 'NONE',  ( -38.70827623999313971, 15.00000000000000355, -151.7039193589360764 ) ) ;
#6146 = PERSON_AND_ORGANIZATION_ROLE ( 'design_supplier' ) ;
#6147 = FACE_OUTER_BOUND ( 'NONE', #5168, .T. ) ;
#6148 = ORIENTED_EDGE ( 'NONE', *, *, #8477, .T. ) ;
#6149 = CARTESIAN_POINT ( 'NONE',  ( 2.298097038856278473, 1.625000000000000222, -5.798097038856279362 ) ) ;
#6150 = CARTESIAN_POINT ( 'NONE',  ( 16.54458777588525820, 8.749999999999998224, -93.72227738972755162 ) ) ;
#6151 = CARTESIAN_POINT ( 'NONE',  ( 2.651650429449553314, 15.37500000000000178, -0.8483495705504476847 ) ) ;
#6152 = CARTESIAN_POINT ( 'NONE',  ( -64.55122089772132199, 14.81922317904516184, -208.3565710730559033 ) ) ;
#6153 = CARTESIAN_POINT ( 'NONE',  ( 14.10364480454416736, 12.78325705495013409, -126.3882374904445953 ) ) ;
#6154 = CARTESIAN_POINT ( 'NONE',  ( -1.346194077712558945, 3.562500000000000888, -0.2500000000000002220 ) ) ;
#6155 = CARTESIAN_POINT ( 'NONE',  ( 10.32514698675680087, 14.49901653209251151, -106.1904513033518356 ) ) ;
#6156 = APPROVAL_STATUS ( 'not_yet_approved' ) ;
#6157 = LOCAL_TIME ( 12, 28, 20.00000000000000000, #8945 ) ;
#6158 = DIRECTION ( 'NONE',  ( 0.000000000000000000, 0.000000000000000000, -1.000000000000000000 ) ) ;
#6159 = CARTESIAN_POINT ( 'NONE',  ( 26.15341798802279527, 4.000000000000000000, -138.7600702976168066 ) ) ;
#6160 = AXIS2_PLACEMENT_3D ( 'NONE', #8274, #7267, #14089 ) ;
#6161 = ORIENTED_EDGE ( 'NONE', *, *, #11493, .F. ) ;
#6162 = CARTESIAN_POINT ( 'NONE',  ( 4.763827962848262487, 0.9384448409284688042, 2.740567078347254881 ) ) ;
#6163 = CARTESIAN_POINT ( 'NONE',  ( 2.298097038856279362, 5.875000000000000000, -1.201902961143720860 ) ) ;
#6164 = CARTESIAN_POINT ( 'NONE',  ( -68.56997004632950166, 9.999999999999998224, -179.5402275981996638 ) ) ;
#6165 = CARTESIAN_POINT ( 'NONE',  ( -3.980102097228897738E-16, 1.000000000000000000, -6.749999999999999112 ) ) ;
#6166 = ADVANCED_FACE ( 'NONE', ( #1016 ), #7694, .T. ) ;
#6167 = CARTESIAN_POINT ( 'NONE',  ( 3.249999999999998224, 6.187500000000001776, -4.846194077712561388 ) ) ;
#6168 = EDGE_CURVE ( 'NONE', #3665, #14503, #12690, .T. ) ;
#6169 = CARTESIAN_POINT ( 'NONE',  ( -0.8648157786182795181, 15.00000000000000000, -108.5968152657687256 ) ) ;
#6170 = CARTESIAN_POINT ( 'NONE',  ( 0.2625675448779599130, 10.37192832877892101, 2.974107436473207411 ) ) ;
#6171 = LOCAL_TIME ( 12, 28, 20.00000000000000000, #15202 ) ;
#6172 = DIRECTION ( 'NONE',  ( 0.8538457527776451839, 0.000000000000000000, 0.5205261093005582040 ) ) ;
#6173 = ADVANCED_FACE ( 'NONE', ( #10290 ), #12842, .T. ) ;
#6174 = CARTESIAN_POINT ( 'NONE',  ( -2.298097038856278918, 3.375000000000000000, -5.798097038856277585 ) ) ;
#6175 = CARTESIAN_POINT ( 'NONE',  ( 2.298097038856278029, 15.12500000000000000, -5.798097038856279362 ) ) ;
#6176 = CIRCLE ( 'NONE', #3463, 0.5000000000000017764 ) ;
#6177 = CARTESIAN_POINT ( 'NONE',  ( 2.651650429449553759, 6.875000000000000000, -0.8483495705504471296 ) ) ;
#6178 = CARTESIAN_POINT ( 'NONE',  ( -4.238936666282000942, 10.20023565101511842, -48.01451400917154899 ) ) ;
#6179 = CARTESIAN_POINT ( 'NONE',  ( 3.749999999999999556, 6.250000000000000888, -3.500000000000000444 ) ) ;
#6180 = CARTESIAN_POINT ( 'NONE',  ( 0.8127647490234470862, 12.34370856009516793, 2.588856853449111650 ) ) ;
#6181 = CARTESIAN_POINT ( 'NONE',  ( 13.09348522998630848, 3.759190269696439657, -166.1421527720724782 ) ) ;
#6182 = CARTESIAN_POINT ( 'NONE',  ( -8.772031809916272849, 1.679412279786333562, -105.4401748263509262 ) ) ;
#6183 = APPROVAL ( #12193, 'UNSPECIFIED' ) ;
#6184 = AXIS2_PLACEMENT_3D ( 'NONE', #9958, #13530, #13455 ) ;
#6185 = DIRECTION ( 'NONE',  ( 0.9961255586397049777, 0.000000000000000000, -0.08794243244723005948 ) ) ;
#6186 = CARTESIAN_POINT ( 'NONE',  ( 9.939878312292615092, 9.999999999999998224, -115.2320631035898373 ) ) ;
#6187 = CIRCLE ( 'NONE', #13845, 14.80000000000025651 ) ;
#6188 = AXIS2_PLACEMENT_3D ( 'NONE', #11745, #2257, #160 ) ;
#6189 = CARTESIAN_POINT ( 'NONE',  ( 8.029176165208181004, 2.106883416375387341, 2.293638343255871348 ) ) ;
#6190 = CARTESIAN_POINT ( 'NONE',  ( 0.3766621274091721538, 0.2615998065109338411, -7.070313984750484337 ) ) ;
#6191 = ORIENTED_EDGE ( 'NONE', *, *, #8081, .F. ) ;
#6192 = CARTESIAN_POINT ( 'NONE',  ( 3.749999999999999112, 8.187500000000000000, -5.053300858899108405 ) ) ;
#6193 = ORIENTED_EDGE ( 'NONE', *, *, #4574, .F. ) ;
#6194 = CARTESIAN_POINT ( 'NONE',  ( -5.763540231018621007, 4.336808689942017736E-16, -109.7236846929783809 ) ) ;
#6195 = CARTESIAN_POINT ( 'NONE',  ( -11.27598888897756346, 0.000000000000000000, -40.77697206847459910 ) ) ;
#6196 = CARTESIAN_POINT ( 'NONE',  ( 1.553300858899108849, 8.937500000000001776, 0.2499999999999993616 ) ) ;
#6197 = CARTESIAN_POINT ( 'NONE',  ( 2.651650429449553314, 7.375000000000000000, -0.8483495705504476847 ) ) ;
#6198 = LINE ( 'NONE', #5960, #12669 ) ;
#6199 = ORIENTED_EDGE ( 'NONE', *, *, #10368, .F. ) ;
#6200 = CARTESIAN_POINT ( 'NONE',  ( -8.195495352952498536, 1.415092730851200020, -116.3141769264971259 ) ) ;
#6201 = CARTESIAN_POINT ( 'NONE',  ( 3.249999999999998224, 4.312500000000000000, -2.153805922287439945 ) ) ;
#6202 = EDGE_CURVE ( 'NONE', #8353, #7290, #8232, .T. ) ;
#6203 = CIRCLE ( 'NONE', #9651, 1.771449424009387208 ) ;
#6204 = CARTESIAN_POINT ( 'NONE',  ( -4.592425496802573972E-16, 11.50000000000000000, -7.249999999999999112 ) ) ;
#6205 = CARTESIAN_POINT ( 'NONE',  ( -63.94155209071244883, 15.00000000000000000, -181.7374336199717959 ) ) ;
#6206 = DIRECTION ( 'NONE',  ( 1.000000000000000000, 0.000000000000000000, 0.000000000000000000 ) ) ;
#6207 = CARTESIAN_POINT ( 'NONE',  ( 25.21562136927963138, -10.21819190899177165, 4.054941874107425015 ) ) ;
#6208 = CARTESIAN_POINT ( 'NONE',  ( -1.346194077712559389, 6.437500000000000888, -6.749999999999999112 ) ) ;
#6209 = DIRECTION ( 'NONE',  ( 0.000000000000000000, 0.000000000000000000, 1.000000000000000000 ) ) ;
#6210 = CALENDAR_DATE ( 2026, 8, 10 ) ;
#6211 = CARTESIAN_POINT ( 'NONE',  ( -5.134731047605749943, 5.000000000000798472, -128.4544621779346585 ) ) ;
#6212 = LINE ( 'NONE', #5059, #3450 ) ;
#6213 = EDGE_LOOP ( 'NONE', ( #8106, #710, #10376, #2461, #4429 ) ) ;
#6214 = CARTESIAN_POINT ( 'NONE',  ( -8.289881740238502772, 2.075239479414269894, -35.21986562831451550 ) ) ;
#6215 = CARTESIAN_POINT ( 'NONE',  ( 3.249999999999999112, 14.81250000000000178, -2.153805922287439945 ) ) ;
#6216 = CIRCLE ( 'NONE', #1281, 3.750000000000003109 ) ;
#6217 = VERTEX_POINT ( 'NONE', #11744 ) ;
#6218 = EDGE_LOOP ( 'NONE', ( #4511, #4584, #4905, #5715 ) ) ;
#6219 = CARTESIAN_POINT ( 'NONE',  ( -1.500000000000000000, 4.500000000000000888, 0.2500000000000002220 ) ) ;
#6220 = CARTESIAN_POINT ( 'NONE',  ( 2.651650429449553314, 11.37500000000000178, -0.8483495705504476847 ) ) ;
#6221 = CARTESIAN_POINT ( 'NONE',  ( 3.249999999999998224, 11.31250000000000355, -2.153805922287439945 ) ) ;
#6222 = CARTESIAN_POINT ( 'NONE',  ( 3.249999999999998224, 10.31250000000000000, -2.153805922287439945 ) ) ;
#6223 = ORIENTED_EDGE ( 'NONE', *, *, #10836, .T. ) ;
#6224 = DIRECTION ( 'NONE',  ( 0.000000000000000000, -0.000000000000000000, 1.000000000000000000 ) ) ;
#6225 = CARTESIAN_POINT ( 'NONE',  ( -3.249999999999999556, 6.312500000000000888, -4.846194077712557835 ) ) ;
#6226 = ADVANCED_FACE ( 'NONE', ( #9283 ), #4573, .T. ) ;
#6227 = PRODUCT ( 'MAS-153', 'MAS-153', '', ( #12236 ) ) ;
#6228 =( GEOMETRIC_REPRESENTATION_CONTEXT ( 3 ) GLOBAL_UNCERTAINTY_ASSIGNED_CONTEXT ( ( #5267 ) ) GLOBAL_UNIT_ASSIGNED_CONTEXT ( ( #6124, #14332, #7281 ) ) REPRESENTATION_CONTEXT ( 'NONE', 'WORKASPACE' ) );
#6229 = CARTESIAN_POINT ( 'NONE',  ( 0.2499999999999999445, 4.500000000000000888, 1.500000000000000222 ) ) ;
#6230 = CARTESIAN_POINT ( 'NONE',  ( 4.033098156699464809, 0.09438068890155107415, -1.663700395152567513 ) ) ;
#6231 = LINE ( 'NONE', #5075, #6702 ) ;
#6232 = PERSON_AND_ORGANIZATION_ROLE ( 'creator' ) ;
#6233 = CARTESIAN_POINT ( 'NONE',  ( -25.07602529789992118, 1.361017155774153053, -206.3226864593361256 ) ) ;
#6234 = ORIENTED_EDGE ( 'NONE', *, *, #8923, .F. ) ;
#6235 = CARTESIAN_POINT ( 'NONE',  ( -3.980102097228897245E-16, 2.500000000000000000, -6.749999999999999112 ) ) ;
#6236 = CARTESIAN_POINT ( 'NONE',  ( 3.749999999999998668, 13.68750000000000000, -5.053300858899107517 ) ) ;
#6237 = FACE_OUTER_BOUND ( 'NONE', #12721, .T. ) ;
#6238 = CARTESIAN_POINT ( 'NONE',  ( 2.651650429449552870, 12.12500000000000000, -6.151650429449553314 ) ) ;
#6239 = AXIS2_PLACEMENT_3D ( 'NONE', #8789, #2918, #4006 ) ;
#6240 = CARTESIAN_POINT ( 'NONE',  ( -65.43041955727726133, 15.34010611920397160, -204.2233706068106187 ) ) ;
#6241 = DIRECTION ( 'NONE',  ( 1.000000000000000000, 0.000000000000000000, 0.000000000000000000 ) ) ;
#6242 = CARTESIAN_POINT ( 'NONE',  ( 3.249999999999999556, 8.750000000000000000, -3.500000000000000000 ) ) ;
#6243 =( BOUNDED_SURFACE ( )  B_SPLINE_SURFACE ( 3, 2, ( 
 ( #8021, #9261, #11724 ),
 ( #12746, #9106, #15233 ),
 ( #8095, #3536, #5622 ),
 ( #7944, #2377, #3383 ),
 ( #11653, #2159, #6861 ),
 ( #10566, #14136, #4625 ),
 ( #11574, #13828, #5702 ),
 ( #12819, #7075, #4698 ),
 ( #10335, #12664, #9336 ),
 ( #2227, #2308, #2080 ),
 ( #11507, #15078, #8169 ),
 ( #12973, #15302, #8245 ),
 ( #6935, #921, #1070 ),
 ( #10421, #11795, #15157 ),
 ( #13914, #1209, #4553 ),
 ( #5779, #10500, #5919 ),
 ( #14059, #3458, #12897 ),
 ( #7009, #1144, #5847 ),
 ( #10873, #13284, #3851 ),
 ( #8316, #7473, #207 ),
 ( #10958, #8548, #377 ),
 ( #2687, #6240, #9724 ),
 ( #9636, #292, #5085 ),
 ( #13207, #5007, #14454 ),
 ( #14370, #1608, #3769 ),
 ( #7386, #12025, #8473 ),
 ( #13042, #9799, #9485 ),
 ( #12108, #14210, #61 ),
 ( #2452, #14529, #1528 ),
 ( #3927, #12190, #8625 ),
 ( #4770, #6152, #10720 ),
 ( #3612, #4846, #3682 ),
 ( #13364, #1295, #7236 ),
 ( #2769, #2610, #10645 ),
 ( #7148, #11871, #5997 ),
 ( #134, #9557, #14282 ),
 ( #8392, #13124, #1447 ),
 ( #2534, #7311, #11948 ),
 ( #1373, #6075, #10793 ),
 ( #4920, #4314, #13592 ) ),
 .UNSPECIFIED., .F., .F., .F. ) 
 B_SPLINE_SURFACE_WITH_KNOTS ( ( 4, 2, 2, 2, 2, 2, 2, 2, 2, 2, 2, 2, 2, 2, 2, 2, 2, 2, 2, 4 ),
 ( 3, 3 ),
 ( -3.279975126961391755E-05, 0.006014536522838872037, 0.009038204659893115181, 0.01206187279694735832, 0.01508554093400159973, 0.01810920907105584288, 0.01962104313958296445, 0.02037696017384652697, 0.02113287720811008602, 0.02188879424237364507, 0.02226675275950542460, 0.02264471127663720759, 0.02302266979376899059, 0.02321164905233488035, 0.02340062831090077011, 0.02358960756946665988, 0.02377858682803254964, 0.02387307645731549452, 0.02396756608659843940, 0.02415654534516432916 ),
 ( 0.000000000000000000, 1.000000000000000000 ),
 .UNSPECIFIED. ) 
 GEOMETRIC_REPRESENTATION_ITEM ( )  RATIONAL_B_SPLINE_SURFACE ( (
 ( 1.000000000000000000, 1.000000000000000000, 1.000000000000000000),
 ( 1.000000000000000000, 0.9998961004008237730, 1.000000000000000000),
 ( 1.000000000000000000, 0.9981490631740187469, 1.000000000000000000),
 ( 1.000000000000000000, 0.9892551553995345692, 1.000000000000000000),
 ( 1.000000000000000000, 0.9852355408993450636, 1.000000000000000000),
 ( 1.000000000000000000, 0.9735752570600945122, 1.000000000000000000),
 ( 1.000000000000000000, 0.9659716152100031872, 1.000000000000000000),
 ( 1.000000000000000000, 0.9442171815146421787, 1.000000000000000000),
 ( 1.000000000000000000, 0.9301391107196244068, 1.000000000000000000),
 ( 1.000000000000000000, 0.8893577403784588276, 1.000000000000000000),
 ( 1.000000000000000000, 0.8629525740881984763, 1.000000000000000000),
 ( 1.000000000000000000, 0.8031463202808644120, 1.000000000000000000),
 ( 1.000000000000000000, 0.7797588792457152973, 1.000000000000000000),
 ( 1.000000000000000000, 0.7364480129656714169, 1.000000000000000000),
 ( 1.000000000000000000, 0.7206346151360477625, 1.000000000000000000),
 ( 1.000000000000000000, 0.6854091271955076170, 1.000000000000000000),
 ( 1.000000000000000000, 0.6659717199882734251, 1.000000000000000000),
 ( 1.000000000000000000, 0.6224610072577244635, 1.000000000000000000),
 ( 1.000000000000000000, 0.5983971201618294433, 1.000000000000000000),
 ( 1.000000000000000000, 0.5574794907613763728, 1.000000000000000000),
 ( 1.000000000000000000, 0.5430094399006958339, 1.000000000000000000),
 ( 1.000000000000000000, 0.5122087497860612348, 1.000000000000000000),
 ( 1.000000000000000000, 0.4959417466219665505, 1.000000000000000000),
 ( 1.000000000000000000, 0.4614524395396406575, 1.000000000000000000),
 ( 1.000000000000000000, 0.4432189288362176072, 1.000000000000000000),
 ( 1.000000000000000000, 0.4143494501494444093, 1.000000000000000000),
 ( 1.000000000000000000, 0.4045375185897135961, 1.000000000000000000),
 ( 1.000000000000000000, 0.3847318188904718661, 1.000000000000000000),
 ( 1.000000000000000000, 0.3747241291590798773, 1.000000000000000000),
 ( 1.000000000000000000, 0.3547825414681071154, 1.000000000000000000),
 ( 1.000000000000000000, 0.3447758195551594018, 1.000000000000000000),
 ( 1.000000000000000000, 0.3258420213088968898, 1.000000000000000000),
 ( 1.000000000000000000, 0.3168993536526623078, 1.000000000000000000),
 ( 1.000000000000000000, 0.3051118154061103760, 1.000000000000000000),
 ( 1.000000000000000000, 0.3014427353064685899, 1.000000000000000000),
 ( 1.000000000000000000, 0.2949341713297093381, 1.000000000000000000),
 ( 1.000000000000000000, 0.2921166433287153419, 1.000000000000000000),
 ( 1.000000000000000000, 0.2851959977589787476, 1.000000000000000000),
 ( 1.000000000000000000, 0.2826324211101104988, 1.000000000000000000),
 ( 1.000000000000000000, 0.2826388035360150597, 1.000000000000000000) ) ) 
 REPRESENTATION_ITEM ( '' )  SURFACE ( )  );
#6244 = CARTESIAN_POINT ( 'NONE',  ( -8.886921396801742645, 2.500000000000000444, -105.5168766094550676 ) ) ;
#6245 = APPROVAL_STATUS ( 'not_yet_approved' ) ;
#6246 = FACE_OUTER_BOUND ( 'NONE', #12423, .T. ) ;
#6247 = CARTESIAN_POINT ( 'NONE',  ( -8.886921396801742645, 9.999999999999998224, -105.5168766094550676 ) ) ;
#6248 = ORIENTED_EDGE ( 'NONE', *, *, #15190, .F. ) ;
#6249 = CARTESIAN_POINT ( 'NONE',  ( 5.592662329148081923, 2.365617111880286672, 4.427078738979575157 ) ) ;
#6250 = CARTESIAN_POINT ( 'NONE',  ( -2.298097038856278473, 5.125000000000000000, -1.201902961143720416 ) ) ;
#6251 = AXIS2_PLACEMENT_3D ( 'NONE', #3846, #6462, #10025 ) ;
#6252 = CARTESIAN_POINT ( 'NONE',  ( -70.11278167081923129, 10.00000000000000355, -193.2159842960370497 ) ) ;
#6253 = CARTESIAN_POINT ( 'NONE',  ( -1.346194077712559389, 12.43750000000000000, -6.749999999999999112 ) ) ;
#6254 = CARTESIAN_POINT ( 'NONE',  ( -3.249999999999999112, 10.81250000000000000, -4.846194077712558723 ) ) ;
#6255 = FACE_OUTER_BOUND ( 'NONE', #3515, .T. ) ;
#6256 = CARTESIAN_POINT ( 'NONE',  ( -2.298097038856278473, 0.1250000000000000000, -1.201902961143720416 ) ) ;
#6257 = CARTESIAN_POINT ( 'NONE',  ( -22.00712180358226533, 15.00000000000000000, -133.4290821151669206 ) ) ;
#6258 = CARTESIAN_POINT ( 'NONE',  ( 3.249999999999999112, 5.812500000000000000, -2.153805922287439945 ) ) ;
#6259 = CARTESIAN_POINT ( 'NONE',  ( 0.000000000000000000, 1.500000000000000222, 0.2499999999999998057 ) ) ;
#6260 = CARTESIAN_POINT ( 'NONE',  ( 1.553300858899108849, 3.937500000000000000, 0.2499999999999993616 ) ) ;
#6261 = CARTESIAN_POINT ( 'NONE',  ( -4.038573370754110492, 10.62993540156934458, -45.72135289039659511 ) ) ;
#6262 = CARTESIAN_POINT ( 'NONE',  ( -1.553300858899107073, 6.937500000000001776, -7.249999999999999112 ) ) ;
#6263 = CIRCLE ( 'NONE', #11923, 3.500000000000003109 ) ;
#6264 = CARTESIAN_POINT ( 'NONE',  ( 3.746804550798221278, 14.90004864566718723, 1.209732483988228191 ) ) ;
#6265 = CIRCLE ( 'NONE', #6509, 5.000000000000000000 ) ;
#6266 = CARTESIAN_POINT ( 'NONE',  ( 11.10165801154622933, 0.7750707670001704130, -165.0650903923130102 ) ) ;
#6267 = LINE ( 'NONE', #5108, #10043 ) ;
#6268 = EDGE_CURVE ( 'NONE', #5826, #2801, #11677, .T. ) ;
#6269 = FACE_OUTER_BOUND ( 'NONE', #13442, .T. ) ;
#6270 = DIRECTION ( 'NONE',  ( 1.420304845956009546E-14, 0.000000000000000000, 1.000000000000000000 ) ) ;
#6271 = CARTESIAN_POINT ( 'NONE',  ( 7.721531454929292160, 1.697151707906022766, 2.086477409661676052 ) ) ;
#6272 = VERTEX_POINT ( 'NONE', #15027 ) ;
#6273 = CARTESIAN_POINT ( 'NONE',  ( -4.592425496802573972E-16, 14.00000000000000000, -7.250000000000000000 ) ) ;
#6274 = ORIENTED_EDGE ( 'NONE', *, *, #6009, .F. ) ;
#6275 = FACE_OUTER_BOUND ( 'NONE', #14362, .T. ) ;
#6276 = CARTESIAN_POINT ( 'NONE',  ( -12.98043033971411120, 4.000000000000098588, -189.9700568513258077 ) ) ;
#6277 = CARTESIAN_POINT ( 'NONE',  ( 0.000000000000000000, 11.00000000000000000, 0.2500000000000002220 ) ) ;
#6278 = AXIS2_PLACEMENT_3D ( 'NONE', #8726, #14625, #5609 ) ;
#6279 = CARTESIAN_POINT ( 'NONE',  ( 3.749999999999999112, 9.312500000000001776, -1.946699141100893149 ) ) ;
#6280 = CARTESIAN_POINT ( 'NONE',  ( 2.530298019944474675, 0.000000000000000000, 0.2330448234422078380 ) ) ;
#6281 = ORIENTED_EDGE ( 'NONE', *, *, #2808, .F. ) ;
#6282 = CARTESIAN_POINT ( 'NONE',  ( -3.249999999999999556, 4.750000000000000000, -3.500000000000000000 ) ) ;
#6283 = CARTESIAN_POINT ( 'NONE',  ( -1.553300858899106629, 9.062499999999998224, 0.2500000000000002220 ) ) ;
#6284 = CARTESIAN_POINT ( 'NONE',  ( -69.91247589395200634, 9.999999999999998224, -187.7969989154814812 ) ) ;
#6285 = DIRECTION ( 'NONE',  ( 0.05964429961207245307, -0.000000000000000000, 0.9982196940171964572 ) ) ;
#6286 = CARTESIAN_POINT ( 'NONE',  ( -1.346194077712559389, 8.437500000000000000, -6.749999999999999112 ) ) ;
#6287 = VECTOR ( 'NONE', #10713, 1000.000000000000000 ) ;
#6288 = CARTESIAN_POINT ( 'NONE',  ( -8.249568998113842255, 15.00000000000488676, -121.3053947661176011 ) ) ;
#6289 = CALENDAR_DATE ( 2026, 8, 10 ) ;
#6290 = EDGE_CURVE ( 'NONE', #5680, #11692, #2067, .T. ) ;
#6291 = CARTESIAN_POINT ( 'NONE',  ( -4.439363805772839733, 8.673617379884035472E-16, -116.8256146818904284 ) ) ;
#6292 = ORIENTED_EDGE ( 'NONE', *, *, #14235, .T. ) ;
#6293 = CARTESIAN_POINT ( 'NONE',  ( 4.554677347145018373, -2.225540348348185052E-17, 1.000000000000000000 ) ) ;
#6294 = CARTESIAN_POINT ( 'NONE',  ( 4.999999999999998224, 0.000000000000000000, -45.97309604003007877 ) ) ;
#6295 = ORIENTED_EDGE ( 'NONE', *, *, #8752, .T. ) ;
#6296 = ORIENTED_EDGE ( 'NONE', *, *, #5808, .F. ) ;
#6297 = CARTESIAN_POINT ( 'NONE',  ( 26.04203104729492679, 0.000000000000000000, 69.41411580402544246 ) ) ;
#6298 = CARTESIAN_POINT ( 'NONE',  ( 2.651650429449552870, 13.12500000000000178, -6.151650429449553314 ) ) ;
#6299 = CARTESIAN_POINT ( 'NONE',  ( -3.980102097228897738E-16, 12.00000000000000178, -6.749999999999999112 ) ) ;
#6300 = CARTESIAN_POINT ( 'NONE',  ( 3.249999999999998224, 12.18750000000000178, -4.846194077712561388 ) ) ;
#6301 = VERTEX_POINT ( 'NONE', #5724 ) ;
#6302 = CARTESIAN_POINT ( 'NONE',  ( -4.869293993583121427, 14.99999999999999822, -118.1204535358624668 ) ) ;
#6303 = CARTESIAN_POINT ( 'NONE',  ( -2.298097038856278473, 8.125000000000000000, -1.201902961143720416 ) ) ;
#6304 = CARTESIAN_POINT ( 'NONE',  ( 4.033098156699464809, 0.09438068890155107415, -1.663700395152567513 ) ) ;
#6305 = CC_DESIGN_DATE_AND_TIME_ASSIGNMENT ( #9769, #5130, ( #10865 ) ) ;
#6306 = CARTESIAN_POINT ( 'NONE',  ( 9.990846742651561030, 12.61469588961295685, -45.61014022669046142 ) ) ;
#6307 = CARTESIAN_POINT ( 'NONE',  ( -61.42357225889784189, 10.00000000000000000, -191.1784762114873217 ) ) ;
#6308 = CARTESIAN_POINT ( 'NONE',  ( -42.66341287047314523, 15.00000000000000355, -153.0322522593145891 ) ) ;
#6309 = PERSON_AND_ORGANIZATION ( #3176, #3020 ) ;
#6310 = EDGE_CURVE ( 'NONE', #5770, #3245, #4417, .T. ) ;
#6311 = CARTESIAN_POINT ( 'NONE',  ( -25.10304974847495885, 1.257220125218194262, -206.1099825640657457 ) ) ;
#6312 = ADVANCED_FACE ( 'NONE', ( #15254 ), #4645, .F. ) ;
#6313 = EDGE_CURVE ( 'NONE', #6350, #8933, #10586, .T. ) ;
#6314 = ORIENTED_EDGE ( 'NONE', *, *, #555, .F. ) ;
#6315 = CARTESIAN_POINT ( 'NONE',  ( -2.298097038856278473, 0.1250000000000000000, -1.201902961143720416 ) ) ;
#6316 = CARTESIAN_POINT ( 'NONE',  ( 0.000000000000000000, 14.00000000000000000, 0.2500000000000002220 ) ) ;
#6317 = ORIENTED_EDGE ( 'NONE', *, *, #2197, .F. ) ;
#6318 = LINE ( 'NONE', #1526, #9205 ) ;
#6319 = CARTESIAN_POINT ( 'NONE',  ( 3.749999999999998668, 2.687500000000000888, -5.053300858899107517 ) ) ;
#6320 = CARTESIAN_POINT ( 'NONE',  ( 7.229479027725716378, 3.133978149981274886, -23.67143487013571956 ) ) ;
#6321 = CARTESIAN_POINT ( 'NONE',  ( -2.326411255686738677, 7.379999999999995453, -43.40791589983918186 ) ) ;
#6322 = CARTESIAN_POINT ( 'NONE',  ( 11.32911568598997398, 4.648160439535026001, -106.8195553340705715 ) ) ;
#6323 = APPROVAL_ROLE ( '' ) ;
#6324 = CARTESIAN_POINT ( 'NONE',  ( -67.62417607549662080, 11.93961266018884260, -203.5750017624773989 ) ) ;
#6325 = DIRECTION ( 'NONE',  ( -0.9982196940171964572, 0.000000000000000000, 0.05964429961207245307 ) ) ;
#6326 = ORIENTED_EDGE ( 'NONE', *, *, #13958, .F. ) ;
#6327 = CARTESIAN_POINT ( 'NONE',  ( 27.03835353835733102, 4.606906972193065997, -138.2189567786153361 ) ) ;
#6328 = CARTESIAN_POINT ( 'NONE',  ( -2.298097038856278473, 7.125000000000000000, -1.201902961143720416 ) ) ;
#6329 = CARTESIAN_POINT ( 'NONE',  ( -9.285933603414314064, 2.500000000000000444, -105.1819416496436759 ) ) ;
#6330 = CARTESIAN_POINT ( 'NONE',  ( -1.346194077712559389, 13.43749999999999822, -6.749999999999999112 ) ) ;
#6331 = CARTESIAN_POINT ( 'NONE',  ( 1.346194077712558279, 12.06250000000000000, -6.750000000000000888 ) ) ;
#6332 = CARTESIAN_POINT ( 'NONE',  ( -7.737061903529485640, 9.999999999999998224, -106.6108512366499923 ) ) ;
#6333 = PLANE ( 'NONE',  #4776 ) ;
#6334 = B_SPLINE_CURVE_WITH_KNOTS ( 'NONE', 3,
 ( #12614, #11598, #1018, #943, #12843, #13780, #720, #3179, #7890, #873 ),
 .UNSPECIFIED., .F., .F.,
 ( 4, 2, 2, 2, 4 ),
 ( 0.000000000000000000, 0.0002702708960404994203, 0.0005405417920809988406, 0.0008108126881214983150, 0.001081083584161997681 ),
 .UNSPECIFIED. ) ;
#6335 = DIRECTION ( 'NONE',  ( 0.000000000000000000, 1.000000000000000000, 0.000000000000000000 ) ) ;
#6336 = CARTESIAN_POINT ( 'NONE',  ( 2.298097038856279362, 3.875000000000000000, -1.201902961143720860 ) ) ;
#6337 = CARTESIAN_POINT ( 'NONE',  ( 1.553300858899105963, 7.062499999999999112, -7.249999999999999112 ) ) ;
#6338 = CARTESIAN_POINT ( 'NONE',  ( 1.553300858899105963, 7.562500000000000000, -7.250000000000000000 ) ) ;
#6339 = CARTESIAN_POINT ( 'NONE',  ( -3.803791538539230022, 10.82342741786251850, -43.84832462749526627 ) ) ;
#6340 = CARTESIAN_POINT ( 'NONE',  ( 3.750000000000000000, 6.312500000000000000, -1.946699141100892705 ) ) ;
#6341 = CARTESIAN_POINT ( 'NONE',  ( 5.000000000000000000, 1.301042606982605321E-15, -45.97309604003012851 ) ) ;
#6342 = CARTESIAN_POINT ( 'NONE',  ( 4.329912723285513465, -2.529993217055220178, -43.25836301743402856 ) ) ;
#6343 = CARTESIAN_POINT ( 'NONE',  ( 1.855481649321436777, 15.00000000000000000, -35.83830032691820122 ) ) ;
#6344 = ADVANCED_FACE ( 'NONE', ( #13856 ), #2499, .T. ) ;
#6345 = CARTESIAN_POINT ( 'NONE',  ( 1.041519256436020280, 6.000000000000000000, -139.4527716894433240 ) ) ;
#6346 = CARTESIAN_POINT ( 'NONE',  ( -6.790153584124027475, 6.000000000000000000, -124.9643354754709748 ) ) ;
#6347 = CARTESIAN_POINT ( 'NONE',  ( -25.27664434398002413, -9.897139991990234887E-31, -198.2936395105848817 ) ) ;
#6348 = ORIENTED_EDGE ( 'NONE', *, *, #5808, .T. ) ;
#6349 = CARTESIAN_POINT ( 'NONE',  ( 2.651650429449552870, 12.12500000000000000, -6.151650429449555091 ) ) ;
#6350 = VERTEX_POINT ( 'NONE', #13541 ) ;
#6351 = CARTESIAN_POINT ( 'NONE',  ( 2.961487585051517879, 2.500000000000000444, 5.117137001352175751 ) ) ;
#6352 = CARTESIAN_POINT ( 'NONE',  ( -28.78613703841196170, 8.673617379884035472E-16, -206.1746911135453786 ) ) ;
#6353 = CARTESIAN_POINT ( 'NONE',  ( -2.651650429449553314, 9.375000000000000000, -6.151650429449552426 ) ) ;
#6354 = CARTESIAN_POINT ( 'NONE',  ( -3.750000000000000000, 8.812500000000001776, -5.053300858899105741 ) ) ;
#6355 = CARTESIAN_POINT ( 'NONE',  ( 8.895558325401111688, 6.000000000000000000, -141.4560052469132643 ) ) ;
#6356 = ORIENTED_EDGE ( 'NONE', *, *, #6009, .T. ) ;
#6357 = CARTESIAN_POINT ( 'NONE',  ( -9.678328886309413903, 4.277268689446015237, -116.3720502296793597 ) ) ;
#6358 = CARTESIAN_POINT ( 'NONE',  ( 2.298097038856279362, 7.375000000000000000, -1.201902961143720860 ) ) ;
#6359 = CARTESIAN_POINT ( 'NONE',  ( 2.651650429449552870, 9.625000000000000000, -6.151650429449554203 ) ) ;
#6360 = CARTESIAN_POINT ( 'NONE',  ( -70.04737159634794352, 14.99999999999942624, -194.4639900967369783 ) ) ;
#6361 = CARTESIAN_POINT ( 'NONE',  ( 30.32986759126112730, 0.000000000000000000, 43.04214087805580391 ) ) ;
#6362 = CARTESIAN_POINT ( 'NONE',  ( 3.249999999999999112, 8.812500000000000000, -2.153805922287439945 ) ) ;
#6363 = CARTESIAN_POINT ( 'NONE',  ( -8.289881740238515206, 2.075239479414269894, -35.21986562831452261 ) ) ;
#6364 = CARTESIAN_POINT ( 'NONE',  ( -6.790153584124027475, 9.999999999999998224, -124.9643354754709748 ) ) ;
#6365 = CARTESIAN_POINT ( 'NONE',  ( 8.769209038263809930, 8.673617379884035472E-16, -110.8932515379864583 ) ) ;
#6366 = DIRECTION ( 'NONE',  ( -0.08794243244722427244, 0.000000000000000000, -0.9961255586397055328 ) ) ;
#6367 = CARTESIAN_POINT ( 'NONE',  ( 5.228075279701640099, 4.000000000000000000, -163.7939279834373849 ) ) ;
#6368 = ORIENTED_EDGE ( 'NONE', *, *, #12686, .F. ) ;
#6369 = DIRECTION ( 'NONE',  ( -0.4304374328763155289, 2.729281898310473032E-15, 0.9026204165532971668 ) ) ;
#6370 = DIRECTION ( 'NONE',  ( 0.000000000000000000, 1.000000000000000000, 0.000000000000000000 ) ) ;
#6371 = CARTESIAN_POINT ( 'NONE',  ( -1.553300858899107073, 10.93750000000000355, -7.249999999999999112 ) ) ;
#6372 = CARTESIAN_POINT ( 'NONE',  ( -1.346194077712559167, 10.93750000000000355, -6.749999999999999112 ) ) ;
#6373 = CARTESIAN_POINT ( 'NONE',  ( 2.298097038856279362, 14.37500000000000000, -1.201902961143720860 ) ) ;
#6374 = VERTEX_POINT ( 'NONE', #14938 ) ;
#6375 = CARTESIAN_POINT ( 'NONE',  ( -3.249999999999999556, 7.312500000000000888, -4.846194077712557835 ) ) ;
#6376 = ADVANCED_FACE ( 'NONE', ( #779 ), #4090, .T. ) ;
#6377 = CARTESIAN_POINT ( 'NONE',  ( -6.790153584124040798, 6.000000000000000000, -124.9643354754709748 ) ) ;
#6378 = DIRECTION ( 'NONE',  ( 0.000000000000000000, 1.000000000000000000, 0.000000000000000000 ) ) ;
#6379 = CARTESIAN_POINT ( 'NONE',  ( 5.841195078839528598, 3.026373079034796465, 4.845806430354895333 ) ) ;
#6380 = CARTESIAN_POINT ( 'NONE',  ( -76.20282042307043469, 10.00000000000000000, -188.4633497277649496 ) ) ;
#6381 = PERSON_AND_ORGANIZATION ( #3176, #3020 ) ;
#6382 = DIRECTION ( 'NONE',  ( -0.08794243244722425856, 0.000000000000000000, -0.9961255586397054218 ) ) ;
#6383 = VERTEX_POINT ( 'NONE', #11131 ) ;
#6384 = CARTESIAN_POINT ( 'NONE',  ( 0.000000000000000000, 9.000000000000001776, -0.2500000000000002220 ) ) ;
#6385 = CARTESIAN_POINT ( 'NONE',  ( -3.249999999999999556, 13.75000000000000000, -3.500000000000000000 ) ) ;
#6386 = CARTESIAN_POINT ( 'NONE',  ( -3.749999999999999556, -0.2499999999999998890, -3.499999999999999112 ) ) ;
#6387 = ORIENTED_EDGE ( 'NONE', *, *, #12736, .T. ) ;
#6388 = CYLINDRICAL_SURFACE ( 'NONE', #10195, 10.00000000000000888 ) ;
#6389 = CARTESIAN_POINT ( 'NONE',  ( 1.553300858899105963, 1.562500000000000000, -7.250000000000000888 ) ) ;
#6390 = EDGE_CURVE ( 'NONE', #10045, #8206, #7743, .T. ) ;
#6391 = DIRECTION ( 'NONE',  ( -0.9997619372588932851, 0.000000000000000000, -0.02181900108494707474 ) ) ;
#6392 = CARTESIAN_POINT ( 'NONE',  ( 0.1753282536233310984, 3.004541188168042609, 1.985946371125043575 ) ) ;
#6393 = CARTESIAN_POINT ( 'NONE',  ( -2.651650429449553314, 2.375000000000000000, -6.151650429449552426 ) ) ;
#6394 = PERSON_AND_ORGANIZATION_ROLE ( 'design_supplier' ) ;
#6395 = CARTESIAN_POINT ( 'NONE',  ( 0.3766621274091715987, -0.2500000000000000000, -0.1347136637304948981 ) ) ;
#6396 = CARTESIAN_POINT ( 'NONE',  ( 9.933893833910557802, 5.000000000000000000, -126.1398084322751885 ) ) ;
#6397 = VERTEX_POINT ( 'NONE', #1781 ) ;
#6398 = CARTESIAN_POINT ( 'NONE',  ( 0.000000000000000000, 7.000000000000000000, -0.2500000000000002220 ) ) ;
#6399 = PLANE ( 'NONE',  #11851 ) ;
#6400 = CARTESIAN_POINT ( 'NONE',  ( -1.346194077712559389, 14.43750000000000000, -6.749999999999999112 ) ) ;
#6401 = CARTESIAN_POINT ( 'NONE',  ( 3.249999999999998224, 9.312500000000000000, -2.153805922287439945 ) ) ;
#6402 = PLANE ( 'NONE',  #4289 ) ;
#6403 = CARTESIAN_POINT ( 'NONE',  ( 11.32016196453114709, 12.84598696167400966, -106.4092894439239956 ) ) ;
#6404 = CARTESIAN_POINT ( 'NONE',  ( -2.298097038856278918, 6.375000000000000888, -5.798097038856277585 ) ) ;
#6405 = CARTESIAN_POINT ( 'NONE',  ( -1.553300858899107073, 5.937500000000000000, -7.249999999999999112 ) ) ;
#6406 = EDGE_CURVE ( 'NONE', #9158, #1308, #3545, .T. ) ;
#6407 = CARTESIAN_POINT ( 'NONE',  ( 0.000000000000000000, 11.00000000000000000, 0.2500000000000002220 ) ) ;
#6408 = LOCAL_TIME ( 12, 28, 20.00000000000000000, #5839 ) ;
#6409 = CARTESIAN_POINT ( 'NONE',  ( 10.97489477031424343, 5.773894334217324342, -44.95261552234883595 ) ) ;
#6410 = CARTESIAN_POINT ( 'NONE',  ( 0.1512094758773736836, 2.824932260968233244, 1.712752529570608306 ) ) ;
#6411 = CARTESIAN_POINT ( 'NONE',  ( -3.750000000000000000, 10.68750000000000178, -1.946699141100893149 ) ) ;
#6412 = CARTESIAN_POINT ( 'NONE',  ( 5.091575966645542017, 10.00000000000000000, -108.2758494551189301 ) ) ;
#6413 = VECTOR ( 'NONE', #9847, 1000.000000000000000 ) ;
#6414 = CARTESIAN_POINT ( 'NONE',  ( 10.60542511503523144, 0.3690892158839738646, -164.4558062555837807 ) ) ;
#6415 = CARTESIAN_POINT ( 'NONE',  ( 4.999884908348398049, 0.09438068890155060231, -1.653151978968578462 ) ) ;
#6416 = CARTESIAN_POINT ( 'NONE',  ( -27.69328214320417914, 3.999999999999152678, -176.5249485101540472 ) ) ;
#6417 = CARTESIAN_POINT ( 'NONE',  ( 4.586756373948227328, 1.218752542932547250E-31, -116.5615908754608085 ) ) ;
#6418 = CARTESIAN_POINT ( 'NONE',  ( -40.71937926015205278, 15.00000000000067324, -157.6611590844978252 ) ) ;
#6419 = APPROVAL_PERSON_ORGANIZATION ( #8308, #12267, #2371 ) ;
#6420 = CARTESIAN_POINT ( 'NONE',  ( 1.553300858899105963, 13.06249999999999822, -7.250000000000000888 ) ) ;
#6421 = ORIENTED_EDGE ( 'NONE', *, *, #6313, .T. ) ;
#6422 = PLANE ( 'NONE',  #7992 ) ;
#6423 = CARTESIAN_POINT ( 'NONE',  ( -1.500000000000000000, 5.000000000000000000, 0.2500000000000002220 ) ) ;
#6424 = CARTESIAN_POINT ( 'NONE',  ( 3.749999999999999112, 7.812500000000000000, -1.946699141100892039 ) ) ;
#6425 = CARTESIAN_POINT ( 'NONE',  ( 3.749999999999998668, 10.18750000000000533, -5.053300858899108405 ) ) ;
#6426 = AXIS2_PLACEMENT_3D ( 'NONE', #6361, #5206, #10291 ) ;
#6427 = DIRECTION ( 'NONE',  ( 0.000000000000000000, 0.000000000000000000, 1.000000000000000000 ) ) ;
#6428 = CARTESIAN_POINT ( 'NONE',  ( 3.249999999999999556, 9.250000000000001776, -3.500000000000000000 ) ) ;
#6429 = CARTESIAN_POINT ( 'NONE',  ( -3.750000000000000000, -0.3124999999999999445, -1.946699141100893149 ) ) ;
#6430 = CARTESIAN_POINT ( 'NONE',  ( 0.000000000000000000, 1.000000000000000000, 0.000000000000000000 ) ) ;
#6431 = VECTOR ( 'NONE', #14580, 1000.000000000000000 ) ;
#6432 = CARTESIAN_POINT ( 'NONE',  ( 28.21756277010331004, 6.321094445766561876, -25.21174485404201704 ) ) ;
#6433 = PERSON_AND_ORGANIZATION ( #3176, #3020 ) ;
#6434 = CARTESIAN_POINT ( 'NONE',  ( -1.346194077712559389, 13.43749999999999822, -6.749999999999999112 ) ) ;
#6435 = AXIS2_PLACEMENT_3D ( 'NONE', #11281, #10273, #6643 ) ;
#6436 = CARTESIAN_POINT ( 'NONE',  ( -8.842600465860288139, 2.529993217055222399, -40.10276331981361153 ) ) ;
#6437 = CIRCLE ( 'NONE', #12606, 3.500000000000003109 ) ;
#6438 = DIRECTION ( 'NONE',  ( 0.1564344650402314796, 0.000000000000000000, 0.9876883405951375483 ) ) ;
#6439 = CARTESIAN_POINT ( 'NONE',  ( 4.739435512632367953, 0.000000000000000000, -107.5260682476390599 ) ) ;
#6440 = CARTESIAN_POINT ( 'NONE',  ( 0.2499999999999999445, 4.500000000000000888, 1.500000000000000222 ) ) ;
#6441 = CARTESIAN_POINT ( 'NONE',  ( 0.5944212552585367293, 0.000000000000000000, -138.5540974747773930 ) ) ;
#6442 = EDGE_LOOP ( 'NONE', ( #214, #2567, #9073 ) ) ;
#6443 = LINE ( 'NONE', #5510, #12771 ) ;
#6444 = CARTESIAN_POINT ( 'NONE',  ( 4.995485589807067583, 4.000000000000000888, -172.1291219214232626 ) ) ;
#6445 = CARTESIAN_POINT ( 'NONE',  ( -3.749999999999999556, 13.75000000000000000, -3.499999999999999112 ) ) ;
#6446 = CARTESIAN_POINT ( 'NONE',  ( -3.980102097228897738E-16, 11.00000000000000178, -6.749999999999999112 ) ) ;
#6447 = CARTESIAN_POINT ( 'NONE',  ( -3.249999999999999112, 12.68750000000000000, -2.153805922287440833 ) ) ;
#6448 = ORIENTED_EDGE ( 'NONE', *, *, #10082, .T. ) ;
#6449 = CIRCLE ( 'NONE', #2256, 5.000000000000000000 ) ;
#6450 = CARTESIAN_POINT ( 'NONE',  ( 3.249999999999999556, 9.750000000000000000, -3.500000000000000000 ) ) ;
#6451 = CARTESIAN_POINT ( 'NONE',  ( 6.122889832264990062, 5.000000000000000888, 5.281130614573720905 ) ) ;
#6452 = CARTESIAN_POINT ( 'NONE',  ( -6.951659142864632379, 14.04257511106687240, -104.5073459644900709 ) ) ;
#6453 = CARTESIAN_POINT ( 'NONE',  ( 5.017237182712672272, 1.294471991313842052, 3.318667728194383049 ) ) ;
#6454 = APPLICATION_PROTOCOL_DEFINITION ( 'international standard', 'config_control_design', 1994, #12422 ) ;
#6455 = EDGE_CURVE ( 'NONE', #2289, #9845, #9231, .T. ) ;
#6456 = DIRECTION ( 'NONE',  ( 0.9997619372588931741, 0.000000000000000000, 0.02181900108494707474 ) ) ;
#6457 = ORIENTED_EDGE ( 'NONE', *, *, #13557, .T. ) ;
#6458 = EDGE_CURVE ( 'NONE', #10548, #7289, #11351, .T. ) ;
#6459 = CARTESIAN_POINT ( 'NONE',  ( 3.249999999999999112, 3.812500000000000000, -2.153805922287439945 ) ) ;
#6460 = CARTESIAN_POINT ( 'NONE',  ( -1.553300858899107295, 13.43749999999999822, -7.250000000000000000 ) ) ;
#6461 = ORIENTED_EDGE ( 'NONE', *, *, #4891, .T. ) ;
#6462 = DIRECTION ( 'NONE',  ( -0.9997619372588932851, 0.000000000000000000, -0.02181900108494707474 ) ) ;
#6463 = B_SPLINE_CURVE_WITH_KNOTS ( 'NONE', 3,
 ( #3363, #12798, #2204, #6911, #14037, #3434, #8145, #4674, #8223, #12954, #10618, #2361, #11776, #7058, #1194, #1732, #4068, #7291, #1430, #6297 ),
 .UNSPECIFIED., .F., .F.,
 ( 4, 2, 2, 2, 2, 2, 2, 2, 2, 4 ),
 ( 0.000000000000000000, 0.005157128052839767690, 0.01031425610567953365, 0.02062851221135907076, 0.03094276831703860267, 0.04125702442271813458, 0.05157128052839766996, 0.06188553663407720534, 0.07219979273975672684, 0.08251404884543626916 ),
 .UNSPECIFIED. ) ;
#6464 = LOCAL_TIME ( 12, 28, 20.00000000000000000, #13449 ) ;
#6465 = CARTESIAN_POINT ( 'NONE',  ( -1.553300858899106629, 1.062500000000000222, 0.2500000000000002220 ) ) ;
#6466 = CARTESIAN_POINT ( 'NONE',  ( -49.26721305452313260, 10.00000000000000178, -156.1716796081737471 ) ) ;
#6467 = CARTESIAN_POINT ( 'NONE',  ( 0.2625675447228704718, 4.835792971051144917, 2.974107434716409148 ) ) ;
#6468 = CARTESIAN_POINT ( 'NONE',  ( 0.000000000000000000, 3.061616997868383018E-17, 0.2500000000000002220 ) ) ;
#6469 = PERSON_AND_ORGANIZATION_ROLE ( 'creator' ) ;
#6470 = FACE_OUTER_BOUND ( 'NONE', #4072, .T. ) ;
#6471 = CARTESIAN_POINT ( 'NONE',  ( 3.902875325215932723, 5.000000000000000000, -114.6800873586639824 ) ) ;
#6472 = APPROVAL_PERSON_ORGANIZATION ( #5317, #1853, #6782 ) ;
#6473 = ORIENTED_EDGE ( 'NONE', *, *, #9323, .T. ) ;
#6474 = EDGE_CURVE ( 'NONE', #4341, #788, #5647, .T. ) ;
#6475 = CARTESIAN_POINT ( 'NONE',  ( 2.298097038856279362, 10.87500000000000178, -1.201902961143720860 ) ) ;
#6476 = EDGE_CURVE ( 'NONE', #5312, #10124, #10203, .T. ) ;
#6477 = CARTESIAN_POINT ( 'NONE',  ( -32.22662898424438538, 9.999999999999998224, -135.0284069691736306 ) ) ;
#6478 = CARTESIAN_POINT ( 'NONE',  ( 1.346194077712561166, 2.437500000000000444, -0.2500000000000011102 ) ) ;
#6479 = CARTESIAN_POINT ( 'NONE',  ( 2.298097038856279362, 12.37500000000000178, -1.201902961143720860 ) ) ;
#6480 = CARTESIAN_POINT ( 'NONE',  ( 13.78275167297412906, 6.000000000000000000, -126.2206732457524794 ) ) ;
#6481 = AXIS2_PLACEMENT_3D ( 'NONE', #1708, #13628, #12297 ) ;
#6482 = LINE ( 'NONE', #12206, #11434 ) ;
#6483 = CARTESIAN_POINT ( 'NONE',  ( 3.249999999999999556, 3.750000000000000000, -3.500000000000000000 ) ) ;
#6484 = CARTESIAN_POINT ( 'NONE',  ( -2.651650429449552870, 6.625000000000000000, -0.8483495705504467965 ) ) ;
#6485 = CARTESIAN_POINT ( 'NONE',  ( -2.651650429449553314, 11.37500000000000000, -6.151650429449552426 ) ) ;
#6486 = PLANE ( 'NONE',  #11125 ) ;
#6487 = CARTESIAN_POINT ( 'NONE',  ( -6.885999823355456684, 0.6080386061245605100, -116.9934166929402153 ) ) ;
#6488 = CARTESIAN_POINT ( 'NONE',  ( -2.651650429449553314, 8.874999999999996447, -6.151650429449552426 ) ) ;
#6489 = CARTESIAN_POINT ( 'NONE',  ( 8.602948156611530450, 9.999999999999998224, -113.5765336190000738 ) ) ;
#6490 = APPROVAL ( #5057, 'UNKNOWN' ) ;
#6491 = FACE_OUTER_BOUND ( 'NONE', #2013, .T. ) ;
#6492 = VECTOR ( 'NONE', #4550, 1000.000000000000000 ) ;
#6493 = CARTESIAN_POINT ( 'NONE',  ( 8.994679575448131459, 0.000000000000000000, 14.93252568749840137 ) ) ;
#6494 = B_SPLINE_CURVE_WITH_KNOTS ( 'NONE', 3,
 ( #5407, #5486, #9039, #14126, #7068, #10204, #10122, #4334, #11787, #14863, #5558, #3158, #4260, #4614, #13692, #10711, #3605, #1284, #5987, #4761, #8307, #13035, #7136, #2443 ),
 .UNSPECIFIED., .F., .F.,
 ( 4, 2, 2, 2, 2, 2, 2, 2, 2, 2, 2, 4 ),
 ( 1.734723475976807094E-18, 0.001351098920114992023, 0.002702197840229982311, 0.005404395680459964622, 0.006755494600574955127, 0.008106593520689946500, 0.01080879136091992924, 0.01215989028103492062, 0.01351098920114990852, 0.01621318704137988953, 0.01891538488160987574, 0.02161758272183985502 ),
 .UNSPECIFIED. ) ;
#6495 = EDGE_CURVE ( 'NONE', #10451, #14561, #8736, .T. ) ;
#6496 = CARTESIAN_POINT ( 'NONE',  ( -17.26415303358039921, 3.151119262966928298E-15, -158.1413053092271070 ) ) ;
#6497 = CARTESIAN_POINT ( 'NONE',  ( 6.770579566034210295, -2.743867526398025447, -34.56909192082981974 ) ) ;
#6498 = DESIGN_CONTEXT ( 'detailed design', #590, 'design' ) ;
#6499 = EDGE_CURVE ( 'NONE', #505, #4779, #5406, .T. ) ;
#6500 = CARTESIAN_POINT ( 'NONE',  ( -34.35934156841198472, 15.00000000000000000, -156.1669470276411289 ) ) ;
#6501 = EDGE_CURVE ( 'NONE', #5223, #8123, #13497, .T. ) ;
#6502 = CARTESIAN_POINT ( 'NONE',  ( 1.553300858899109516, 13.43750000000000178, 0.2499999999999993616 ) ) ;
#6503 = VERTEX_POINT ( 'NONE', #2312 ) ;
#6504 = DIRECTION ( 'NONE',  ( -0.000000000000000000, 1.000000000000000000, -0.000000000000000000 ) ) ;
#6505 = CARTESIAN_POINT ( 'NONE',  ( 8.475206276408092876, -1.020558061026469288, -34.56909192082981974 ) ) ;
#6506 = CARTESIAN_POINT ( 'NONE',  ( -3.750000000000000000, 6.687500000000000888, -1.946699141100893149 ) ) ;
#6507 = DIRECTION ( 'NONE',  ( -1.076984184057255207E-17, 1.000000000000000000, -1.219901976936984353E-16 ) ) ;
#6508 = CARTESIAN_POINT ( 'NONE',  ( 2.298097038856278029, 8.125000000000000000, -5.798097038856279362 ) ) ;
#6509 = AXIS2_PLACEMENT_3D ( 'NONE', #7452, #7368, #2898 ) ;
#6510 = CARTESIAN_POINT ( 'NONE',  ( -15.73004658022870927, 0.000000000000000000, -131.7446186346720367 ) ) ;
#6511 = CARTESIAN_POINT ( 'NONE',  ( -3.749999999999999556, 12.31250000000000000, -5.053300858899104853 ) ) ;
#6512 = DIRECTION ( 'NONE',  ( -0.9961255586397050887, 0.000000000000000000, 0.08794243244723005948 ) ) ;
#6513 = CARTESIAN_POINT ( 'NONE',  ( 0.000000000000000000, 0.000000000000000000, 0.000000000000000000 ) ) ;
#6514 = SECURITY_CLASSIFICATION_LEVEL ( 'unclassified' ) ;
#6515 = CARTESIAN_POINT ( 'NONE',  ( -3.249999999999999556, 12.31250000000000000, -4.846194077712557835 ) ) ;
#6516 = CARTESIAN_POINT ( 'NONE',  ( -5.192805064198273257, 10.00000000000000178, -111.6595894180993582 ) ) ;
#6517 = DIRECTION ( 'NONE',  ( 0.000000000000000000, -1.000000000000000000, 0.000000000000000000 ) ) ;
#6518 = CARTESIAN_POINT ( 'NONE',  ( 8.425472749275192186, 2.176832918059240114E-13, -115.5475827924868071 ) ) ;
#6519 = AXIS2_PLACEMENT_3D ( 'NONE', #8566, #7328, #12040 ) ;
#6520 = CARTESIAN_POINT ( 'NONE',  ( 2.543998210651924552, 5.000000000000000888, -136.5336064733039620 ) ) ;
#6521 = AXIS2_PLACEMENT_3D ( 'NONE', #1657, #6370, #883 ) ;
#6522 = CARTESIAN_POINT ( 'NONE',  ( -17.32624372123753886, 9.999999999999998224, -129.3796757791584753 ) ) ;
#6523 = ORIENTED_EDGE ( 'NONE', *, *, #2156, .F. ) ;
#6524 = CARTESIAN_POINT ( 'NONE',  ( -9.240119717576689595, 9.999999999999998224, -104.6630069175297564 ) ) ;
#6525 = DIRECTION ( 'NONE',  ( 0.000000000000000000, -0.000000000000000000, 1.000000000000000000 ) ) ;
#6526 = CARTESIAN_POINT ( 'NONE',  ( 2.651650429449552870, 15.12500000000000000, -6.151650429449553314 ) ) ;
#6527 = CARTESIAN_POINT ( 'NONE',  ( 3.249999999999998224, 10.18750000000000533, -4.846194077712561388 ) ) ;
#6528 = APPROVAL ( #6156, 'UNSPECIFIED' ) ;
#6529 = CARTESIAN_POINT ( 'NONE',  ( 1.346194077712561166, 13.43750000000000178, -0.2500000000000011102 ) ) ;
#6530 = ORIENTED_EDGE ( 'NONE', *, *, #14256, .F. ) ;
#6531 = CARTESIAN_POINT ( 'NONE',  ( -3.249999999999999556, 10.31250000000000000, -4.846194077712557835 ) ) ;
#6532 = AXIS2_PLACEMENT_3D ( 'NONE', #5769, #1138, #7138 ) ;
#6533 = CARTESIAN_POINT ( 'NONE',  ( 12.76858567064540217, 3.999999999993260502, -166.6103056774037441 ) ) ;
#6534 = CARTESIAN_POINT ( 'NONE',  ( 9.948235151679879706, 12.61502403974950326, -43.65837861547728238 ) ) ;
#6535 = DIRECTION ( 'NONE',  ( -0.08794243244722425856, -0.000000000000000000, -0.9961255586397054218 ) ) ;
#6536 = DIRECTION ( 'NONE',  ( -0.000000000000000000, 1.000000000000000000, -0.000000000000000000 ) ) ;
#6537 = APPROVAL_DATE_TIME ( #1826, #3278 ) ;
#6538 = CARTESIAN_POINT ( 'NONE',  ( 8.330271663116334935, 14.99999999999953282, -113.1592731357334003 ) ) ;
#6539 = VERTEX_POINT ( 'NONE', #3386 ) ;
#6540 = CARTESIAN_POINT ( 'NONE',  ( -3.249999999999999556, 6.250000000000000000, -3.499999999999999556 ) ) ;
#6541 = CARTESIAN_POINT ( 'NONE',  ( -24.38883959582580729, 4.000000000000000888, -168.5529178378782262 ) ) ;
#6542 = CARTESIAN_POINT ( 'NONE',  ( -2.651650429449553314, 1.874999999999999778, -6.151650429449552426 ) ) ;
#6543 = ORIENTED_EDGE ( 'NONE', *, *, #11272, .F. ) ;
#6544 = CARTESIAN_POINT ( 'NONE',  ( 4.492499072540838689, 5.000000000000000000, -2.611025101989581820 ) ) ;
#6545 = EDGE_CURVE ( 'NONE', #14298, #11802, #12188, .T. ) ;
#6546 = CARTESIAN_POINT ( 'NONE',  ( -1.553300858899107295, 0.4375000000000000555, -7.250000000000000000 ) ) ;
#6547 = CARTESIAN_POINT ( 'NONE',  ( -60.91137729732987793, 10.00000000000000178, -175.0198515626273661 ) ) ;
#6548 = CARTESIAN_POINT ( 'NONE',  ( 0.2167269470765707806, 3.467221422101828043, 2.454870137451500067 ) ) ;
#6549 = CARTESIAN_POINT ( 'NONE',  ( 2.651650429449552870, 1.625000000000000222, -6.151650429449554203 ) ) ;
#6550 = PERSON_AND_ORGANIZATION_ROLE ( 'classification_officer' ) ;
#6551 = CARTESIAN_POINT ( 'NONE',  ( -4.946131244327882648, 0.4878928319774004096, -1.000000000000001554 ) ) ;
#6552 = DIRECTION ( 'NONE',  ( -0.000000000000000000, -1.000000000000000000, -0.000000000000000000 ) ) ;
#6553 = VERTEX_POINT ( 'NONE', #2162 ) ;
#6554 = CARTESIAN_POINT ( 'NONE',  ( 3.230086961373112242, 9.999999999999998224, 5.208283729180105404 ) ) ;
#6555 = CARTESIAN_POINT ( 'NONE',  ( -2.298097038856279362, 2.875000000000000000, -5.798097038856278473 ) ) ;
#6556 = CARTESIAN_POINT ( 'NONE',  ( -2.298097038856279362, 12.87500000000000000, -5.798097038856278473 ) ) ;
#6557 = CARTESIAN_POINT ( 'NONE',  ( -8.241439964509023497, 9.999999999999998224, -106.0832790697715495 ) ) ;
#6558 =( BOUNDED_SURFACE ( )  B_SPLINE_SURFACE ( 3, 2, ( 
 ( #753, #3297, #6256, #6700, #10972, #4383, #14545, #3941, #13812, #3212, #7931, #12650, #6776, #8642, #11491, #908, #5176, #15287, #12804, #11637, #5901, #2209, #6917, #8151, #4610, #3368, #14120, #14273, #12880, #10485, #2141, #9472, #10409, #15220, #6996, #3521, #4536, #14199, #10705, #3672, #12730, #3602, #5683, #1199, #13031, #10624, #11854, #5762, #8229, #6845, #2366, #1055, #4835, #9320, #11783, #8303, #9249, #122, #14042, #12959, #3440, #2292, #11712, #1130, #11559, #7063, #7131, #5833, #10554, #5983, #975, #4679, #9393, #47, #4757, #2438, #15141, #1278, #13973, #8079, #9547, #9705, #277, #197, #14353, #3835, #4991, #10942, #6062, #7297, #14438, #10780, #5071, #12010, #1359, #8458, #9784, #9619, #1593, #3752, #12089, #6225, #12253, #1436, #8536, #1663, #5227, #7458, #2674, #11020, #2598, #437, #8376, #358, #6142, #10856, #506, #6375, #11088, #13269, #9934, #7374, #8612, #4907, #14516, #14670, #13189, #12174, #3915, #1514, #6303, #13346, #2756, #5145, #8696, #2520, #13105, #2835, #9856, #7216, #11935, #14589, #3993, #13431, #7536, #12320, #736, #2903, #12478, #10305, #12632, #588, #10012, #14896, #14972, #7606, #6450, #5440, #5300, #2044, #4366, #11244, #6606, #2975, #13795, #6531, #7686, #1819, #10161, #6756, #4293, #11395, #14819, #8997, #10085, #889, #663, #12398, #14747, #5369, #4216, #8922, #13573, #13725, #13650, #3124, #3052, #4147, #3193, #7838, #11468, #12552, #5590, #7763, #8775, #1895, #1964, #7906, #8845, #11315, #9075, #6679, #815, #5517, #10239, #4073, #11166, #13507, #1737, #8131, #3273, #3583, #1035, #15043, #4739, #9453, #14179, #10535, #1111, #4436, #13013, #6977, #5815, #11693, #10460, #3419, #15121, #14098, #3502, #4514, #15268, #956, #8209, #5661, #12858, #6895, #2416, #7986, #8283, #5741, #9147 ),
 ( #7112, #13874, #11833, #4659, #4590, #12706, #24, #2120, #9223, #7046, #8059, #2272, #9368, #11615, #1258, #5964, #12940, #6825, #15198, #11541, #10383, #2348, #9297, #11761, #14022, #12784, #13951, #3348, #1181, #2191, #5883, #10603, #9599, #3891, #178, #4887, #6119, #2578, #1339, #12068, #12232, #10832, #8435, #103, #7432, #8354, #13168, #4966, #1487, #2497, #12151, #8673, #1643, #10685, #1569, #3652, #14494, #10996, #8591, #9836, #3729, #6201, #4816, #335, #14327, #2811, #7278, #9764, #6282, #7194, #13406, #11991, #10918, #1414, #251, #9682, #14413, #9529, #5049, #5121, #3812, #8515, #3968, #14250, #13249, #2653, #7355, #13324, #2729, #13082, #413, #11914, #6042, #14568, #7513, #10761, #13485, #12301, #1798, #2953, #8901, #4047, #5278, #13553, #8754, #3032, #9988, #14649, #14726, #7742, #6358, #11294, #11148, #13777, #7662, #5420, #1945, #2884, #4348, #567, #12459, #12377, #6508, #11224, #8826, #11070, #1877, #794, #642, #4125, #14953, #9916, #14800, #13631, #5348, #715, #10064, #7584, #8977, #1714, #6428, #4273, #4194, #6583, #10138, #14876, #13707, #3106, #7817, #12529, #6658, #11371, #5498, #10219, #9055, #3172, #7885, #12609, #487, #5202, #3251, #5642, #939, #3480, #10516, #9351, #8189, #6878, #6734, #14004, #4570, #3330, #11593, #6954, #3402, #3557, #5864, #869, #4720, #9279, #1012, #11447, #2329, #5572, #11523, #14076, #10358, #5720, #8111, #13932, #9431, #14157, #10440, #8263, #2174, #10287, #10583, #12838, #8039, #15251, #9202, #15099, #760, #7028, #1090, #13853, #2251, #2100, #4494, #4642, #6807, #12765, #15177, #11672, #7963, #5796, #2024, #12915, #11741, #15023, #1161, #4414, #9123, #12685, #3787, #4793, #9744, #10976, #3944, #12992, #3868, #5941, #1464, #13302, #6175, #12130, #8570, #10664, #10895, #2705, #311 ),
 ( #4864, #12043, #7405, #9506, #393, #7170, #14388, #9576, #14303, #13144, #155, #2396, #8494, #1546, #3703, #11890, #6259, #1232, #6095, #4941, #8412, #7332, #2554, #80, #5025, #14230, #3632, #14472, #7255, #11972, #8334, #13059, #1392, #10810, #226, #2473, #1313, #9657, #6019, #13225, #10740, #2630, #5102, #9816, #14549, #7092, #11813, #12284, #7565, #10114, #1856, #695, #14855, #13536, #13382, #5329, #11201, #9965, #2935, #13611, #10041, #10197, #12506, #7490, #11344, #623, #7639, #2788, #8953, #12209, #2866, #5400, #1694, #12355, #14778, #5255, #772, #5479, #1775, #14930, #8806, #1624, #1925, #4175, #14705, #6561, #542, #6405, #6637, #13685, #7720, #5180, #8879, #8730, #11124, #11274, #13463, #4105, #6484, #3013, #14628, #12434, #8646, #4253, #3082, #6337, #7796, #11051, #467, #9890, #4025, #11425, #1068, #2305, #10564, #4327, #15231, #13912, #988, #2155, #2223, #3229, #13984, #7942, #8091, #9030, #7864, #8167, #5620, #13755, #9334, #14055, #3455, #15154, #5699, #3150, #7007, #11571, #10419, #4551, #15074, #8019, #4395, #3380, #12817, #6859, #12895, #12662, #10334, #11722, #1142, #6933, #3310, #11650, #13825, #5775, #12583, #9259, #2078, #6790, #5845, #1999, #6712, #919, #847, #4471, #10498, #5549, #4622, #10265, #14997, #9103, #11503, #9181, #12744, #11869, #12971, #1208, #291, #9409, #3848, #9722, #9483, #4693, #14134, #14369, #6238, #10718, #10791, #8242, #11946, #3534, #8390, #15300, #8547, #11793, #5916, #206, #10871, #2375, #7073, #1370, #10641, #13283, #5005, #7145, #2531, #14207, #14453, #2450, #3610, #13040, #6074, #2685, #4919, #7309, #131, #9634, #5995, #12106, #1291, #8314, #59, #4842, #9555, #14280, #3680, #3767, #13122, #8472, #7232, #4768, #7384, #13204, #1527, #2609, #12024, #1445, #6151, #8709, #14762 ),
 ( #12336, #10957, #607, #450, #3068, #2850, #10026, #6546, #2768, #8940, #5159, #1756, #7550, #12268, #11102, #13446, #376, #6465, #5385, #1676, #9872, #4235, #14528, #4087, #2919, #6389, #5314, #523, #3926, #13591, #12189, #13362, #8863, #5238, #9947, #7471, #1607, #14686, #8790, #13521, #8624, #14607, #7620, #6319, #11180, #4008, #11033, #4161, #2994, #7702, #12414, #1838, #11258, #680, #10100, #14837, #13668, #7780, #12495, #5084, #1912, #9797, #7932, #909, #11560, #3298, #8154, #10488, #5464, #9321, #13901, #11492, #11332, #6919, #10181, #831, #13974, #14987, #10324, #8008, #3214, #14044, #3441, #15063, #12882, #6777, #14915, #15221, #12732, #12652, #15144, #13813, #4384, #4611, #11640, #5685, #3139, #9171, #6701, #5537, #4539, #11414, #10256, #2064, #5611, #12571, #2143, #6625, #4459, #9092, #755, #3369, #4313, #6846, #976, #10410, #13741, #8080, #9017, #7853, #1985, #12805, #9250, #2210, #1057, #5763, #12069, #5122, #11784, #9837, #2293, #5050, #1415, #6121, #9917, #488, #5203, #14415, #14650, #3813, #2730, #9396, #336, #4050, #3522, #6283, #9765, #12960, #1570, #8517, #15288, #8230, #2813, #11713, #6359, #12233, #10834, #6997, #1132, #10999, #8756, #13251, #13327, #10555, #14495, #5835, #10919, #4681, #11071, #14122, #2367, #7435, #13408, #7065, #253, #3892, #4968, #9683, #7514, #2655, #8592, #7356, #1645, #1489, #6204, #12153, #414, #14569, #3969, #8675, #8903, #14878, #4197, #10289, #5351, #1800, #9990, #6511, #13633, #11226, #7664, #3108, #14802, #13709, #3034, #4126, #7888, #7819, #6736, #12533, #11451, #12461, #2885, #645, #1947, #12611, #14728, #7745, #9057, #1879, #10140, #11296, #11373, #12379, #6660, #10066, #798, #13486, #1715, #2026, #6586, #7586, #3175, #871, #5574, #8980, #4275, #12302, #15026, #5422, #5500 ),
 ( #10222, #717, #14955, #6429, #4349, #2955, #4416, #13778, #11149, #568, #5280, #8827, #13554, #10518, #1015, #5723, #9282, #11596, #9127, #15253, #3561, #10442, #8041, #2399, #12688, #2253, #1093, #15180, #3482, #4572, #2102, #11743, #10362, #11525, #7030, #14006, #3404, #941, #15102, #8113, #12841, #11675, #6809, #12767, #6958, #5644, #5798, #2176, #4496, #9204, #4644, #13934, #2332, #3332, #6880, #9353, #10585, #1163, #5866, #3, #14079, #13855, #8191, #12918, #4722, #9434, #14160, #8266, #10668, #12995, #7965, #11816, #7095, #1236, #3254, #5944, #84, #14306, #12133, #13148, #8497, #12046, #1395, #12212, #7493, #13231, #1627, #4945, #8337, #13386, #10898, #10813, #13306, #11975, #2557, #8652, #5105, #3872, #1317, #7335, #4867, #3707, #2708, #9579, #8415, #229, #6098, #10743, #6179, #6340, #9660, #7260, #9509, #1549, #2477, #14392, #3790, #314, #11894, #6262, #2791, #11054, #4796, #10979, #13062, #8573, #9820, #7411, #3948, #2633, #5028, #14233, #14552, #3635, #7173, #9747, #14475, #6022, #158, #1466, #396, #7725, #11206, #4180, #546, #14861, #4257, #13617, #4332, #4109, #6488, #9036, #12590, #8959, #10047, #3086, #9970, #7801, #471, #3018, #14709, #8810, #7868, #13760, #3156, #12362, #2007, #1780, #700, #7569, #12439, #6718, #1698, #13689, #1860, #11130, #12514, #628, #13467, #6411, #778, #9895, #5184, #10202, #13540, #14631, #4030, #1930, #8734, #5333, #11279, #2870, #6567, #12288, #8885, #5259, #2939, #7644, #14783, #5405, #11350, #10120, #6642, #5484, #14936, #4700, #11726, #3314, #13988, #10338, #5849, #13917, #15080, #9185, #8097, #9413, #6937, #3460, #6863, #12822, #2161, #8247, #8025, #4475, #7947, #12749, #11576, #993, #5625, #1073, #5704, #11655, #10423, #2082, #10568, #5781, #14138, #10502, #3538, #15159, #852 ),
 ( #2230, #12666, #4627, #6795, #4555, #9264, #12899, #9338, #8171, #2310, #3385, #15236, #14061, #12975, #7011, #1146, #11509, #15304, #2379, #11430, #5555, #10270, #15003, #4399, #9108, #925, #13831, #3234, #3853, #4922, #8550, #13126, #7077, #10722, #13209, #14456, #8318, #8393, #294, #2536, #10795, #1375, #7313, #11873, #3771, #1297, #2612, #11797, #4772, #13286, #14284, #1211, #2689, #7388, #12110, #8475, #9638, #5921, #10647, #14372, #12027, #1449, #7238, #209, #5998, #6154, #10875, #5009, #63, #3684, #11950, #9487, #14212, #9726, #3614, #13044, #6077, #2454, #7150, #136, #4848, #9559, #13028, #3599, #8300, #2206, #2434, #6913, #5830, #12726, #3436, #7128, #6841, #9387, #8147, #972, #4676, #11634, #3292, #11556, #5898, #15059, #9469, #43, #15138, #10320, #4453, #14117, #11849, #1052, #1127, #13894, #2288, #9167, #14039, #5606, #14195, #2137, #5679, #10551, #1196, #8004, #10406, #6993, #4533, #9244, #10620, #12800, #12877, #13970, #4753, #8076, #3365, #5759, #11709, #10481, #15284, #12956, #15216, #4607, #9317, #3518, #8226, #2363, #7060, #11779, #12007, #13186, #3831, #14270, #194, #8455, #3669, #13266, #4904, #9544, #1355, #2671, #2517, #9780, #7212, #9616, #14347, #2751, #14512, #8609, #7455, #6139, #5979, #7371, #8532, #2593, #10853, #6222, #12086, #2832, #5142, #118, #3988, #1510, #272, #10702, #1590, #4832, #10777, #13343, #3749, #4987, #10938, #7294, #8693, #13428, #9702, #7533, #1433, #8372, #9853, #355, #14435, #3912, #5068, #12172, #14586, #6300, #11017, #13101, #432, #6059, #1275, #11931, #1735, #6447, #7683, #4144, #2901, #13648, #13793, #12396, #10010, #1660, #8995, #9932, #14744, #6529, #3050, #4071, #13723, #10237, #3191, #12250, #3122, #5222, #734, #12550, #5438, #11391, #5298, #7761, #6373, #1893, #11164 ),
 ( #586, #8843, #8919, #5515, #12475, #4291, #1817, #6603, #2971, #9072, #13570, #11242, #8772, #661, #5366, #10083, #14817, #11312, #4214, #10158, #14893, #4364, #14970, #11086, #7836, #504, #1961, #6677, #13505, #813, #14667, #7603, #12317, #4665, #6981, #5745, #4520, #15273, #106, #9303, #11621, #3276, #10607, #11544, #1038, #8135, #9373, #5666, #31, #11839, #4819, #13881, #4742, #6828, #2352, #14183, #7050, #13018, #6900, #14105, #7989, #3505, #3353, #5968, #10467, #12944, #9457, #10391, #1263, #8064, #8213, #15201, #4594, #14026, #3423, #12713, #11765, #8289, #12864, #12788, #7116, #2125, #11697, #5818, #2276, #1185, #1116, #959, #5887, #15125, #9227, #3587, #10538, #2420, #13956, #2193, #10688, #6125, #12072, #7198, #8441, #1420, #11917, #6208, #13172, #2503, #9604, #10923, #10766, #2735, #181, #2581, #7282, #11004, #7441, #1573, #418, #14419, #14258, #340, #1496, #10839, #3817, #14498, #5055, #11074, #13414, #8358, #12237, #9768, #8521, #3657, #9841, #13086, #3734, #6286, #11995, #13254, #3897, #258, #1649, #6362, #2659, #491, #9686, #1343, #4971, #12157, #7360, #8596, #2817, #14572, #13330, #6046, #5128, #14333, #3974, #8679, #4893, #7518, #9532, #12384, #11153, #6591, #6741, #650, #2958, #9921, #1950, #2889, #7669, #14805, #11300, #12306, #6663, #3180, #11454, #5208, #11378, #13491, #8983, #5503, #13712, #4352, #13559, #721, #14653, #10146, #9996, #12615, #1805, #4278, #802, #1719, #7891, #14732, #5425, #6515, #11229, #5354, #10070, #4057, #14881, #14958, #4201, #4131, #13781, #8760, #13636, #12464, #8907, #3111, #3038, #7591, #7822, #6434, #573, #12538, #7748, #1882, #5284, #8831, #10225, #9060, #2029, #13859, #15308, #8251, #3257, #13047, #4705, #9132, #1149, #2458, #2106, #9562, #7015, #9417, #14141, #2540, #14287 ) ),
 .UNSPECIFIED., .T., .F., .T. ) 
 B_SPLINE_SURFACE_WITH_KNOTS ( ( 4, 3, 4 ),
 ( 3, 2, 2, 2, 2, 2, 2, 2, 2, 2, 2, 2, 2, 2, 2, 2, 2, 2, 2, 2, 2, 2, 2, 2, 2, 2, 2, 2, 2, 2, 2, 2, 2, 2, 2, 2, 2, 2, 2, 2, 2, 2, 2, 2, 2, 2, 2, 2, 2, 2, 2, 2, 2, 2, 2, 2, 2, 2, 2, 2, 2, 2, 2, 2, 2, 2, 2, 2, 2, 2, 2, 2, 2, 2, 2, 2, 2, 2, 2, 2, 2, 2, 2, 2, 2, 2, 2, 2, 2, 2, 2, 2, 2, 2, 2, 2, 2, 2, 2, 2, 2, 2, 2, 2, 2, 2, 2, 2, 2, 2, 2, 2, 2, 2, 2, 2, 2, 2, 2, 2, 3 ),
 ( 0.000000000000000000, 0.5000000000000000000, 1.000000000000000000 ),
 ( 0.000000000000000000, 0.008333333333333333218, 0.01666666666666666644, 0.02500000000000000139, 0.03333333333333333287, 0.04166666666666666435, 0.05000000000000000278, 0.05833333333333333426, 0.06666666666666666574, 0.07499999999999999722, 0.08333333333333332871, 0.09166666666666666019, 0.1000000000000000056, 0.1083333333333333370, 0.1166666666666666685, 0.1250000000000000000, 0.1333333333333333315, 0.1416666666666666630, 0.1499999999999999944, 0.1583333333333333259, 0.1666666666666666574, 0.1749999999999999889, 0.1833333333333333204, 0.1916666666666666519, 0.2000000000000000111, 0.2083333333333333426, 0.2166666666666666741, 0.2250000000000000056, 0.2333333333333333370, 0.2416666666666666685, 0.2500000000000000000, 0.2583333333333333037, 0.2666666666666666630, 0.2750000000000000222, 0.2833333333333333259, 0.2916666666666666852, 0.2999999999999999889, 0.3083333333333333481, 0.3166666666666666519, 0.3250000000000000111, 0.3333333333333333148, 0.3416666666666666741, 0.3499999999999999778, 0.3583333333333333370, 0.3666666666666666408, 0.3750000000000000000, 0.3833333333333333037, 0.3916666666666666630, 0.4000000000000000222, 0.4083333333333333259, 0.4166666666666666852, 0.4249999999999999889, 0.4333333333333333481, 0.4416666666666666519, 0.4500000000000000111, 0.4583333333333333148, 0.4666666666666666741, 0.4749999999999999778, 0.4833333333333333370, 0.4916666666666666408, 0.5000000000000000000, 0.5083333333333333037, 0.5166666666666666075, 0.5250000000000000222, 0.5333333333333333259, 0.5416666666666666297, 0.5500000000000000444, 0.5583333333333333481, 0.5666666666666666519, 0.5749999999999999556, 0.5833333333333333703, 0.5916666666666666741, 0.5999999999999999778, 0.6083333333333332815, 0.6166666666666666963, 0.6250000000000000000, 0.6333333333333333037, 0.6416666666666666075, 0.6500000000000000222, 0.6583333333333333259, 0.6666666666666666297, 0.6750000000000000444, 0.6833333333333333481, 0.6916666666666666519, 0.6999999999999999556, 0.7083333333333333703, 0.7166666666666666741, 0.7249999999999999778, 0.7333333333333332815, 0.7416666666666666963, 0.7500000000000000000, 0.7583333333333333037, 0.7666666666666666075, 0.7750000000000000222, 0.7833333333333333259, 0.7916666666666666297, 0.8000000000000000444, 0.8083333333333333481, 0.8166666666666666519, 0.8249999999999999556, 0.8333333333333333703, 0.8416666666666666741, 0.8499999999999999778, 0.8583333333333332815, 0.8666666666666666963, 0.8750000000000000000, 0.8833333333333333037, 0.8916666666666666075, 0.9000000000000000222, 0.9083333333333333259, 0.9166666666666666297, 0.9249999999999999334, 0.9333333333333333481, 0.9416666666666666519, 0.9499999999999999556, 0.9583333333333333703, 0.9666666666666666741, 0.9749999999999999778, 0.9833333333333332815, 0.9916666666666666963, 1.000000000000000000 ),
 .UNSPECIFIED. ) 
 GEOMETRIC_REPRESENTATION_ITEM ( )  RATIONAL_B_SPLINE_SURFACE ( (
 ( 1.000000000000000000, 0.9238795325112867385, 1.000000000000000000, 0.9238795325112867385, 1.000000000000000000, 0.9238795325112867385, 1.000000000000000000, 0.9238795325112867385, 1.000000000000000000, 0.9238795325112867385, 1.000000000000000000, 0.9238795325112867385, 1.000000000000000000, 0.9238795325112867385, 1.000000000000000000, 0.9238795325112867385, 1.000000000000000000, 0.9238795325112867385, 1.000000000000000000, 0.9238795325112867385, 1.000000000000000000, 0.9238795325112867385, 1.000000000000000000, 0.9238795325112867385, 1.000000000000000000, 0.9238795325112867385, 1.000000000000000000, 0.9238795325112867385, 1.000000000000000000, 0.9238795325112867385, 1.000000000000000000, 0.9238795325112867385, 1.000000000000000000, 0.9238795325112867385, 1.000000000000000000, 0.9238795325112867385, 1.000000000000000000, 0.9238795325112867385, 1.000000000000000000, 0.9238795325112867385, 1.000000000000000000, 0.9238795325112867385, 1.000000000000000000, 0.9238795325112867385, 1.000000000000000000, 0.9238795325112867385, 1.000000000000000000, 0.9238795325112867385, 1.000000000000000000, 0.9238795325112867385, 1.000000000000000000, 0.9238795325112867385, 1.000000000000000000, 0.9238795325112867385, 1.000000000000000000, 0.9238795325112867385, 1.000000000000000000, 0.9238795325112867385, 1.000000000000000000, 0.9238795325112867385, 1.000000000000000000, 0.9238795325112867385, 1.000000000000000000, 0.9238795325112867385, 1.000000000000000000, 0.9238795325112867385, 1.000000000000000000, 0.9238795325112867385, 1.000000000000000000, 0.9238795325112867385, 1.000000000000000000, 0.9238795325112867385, 1.000000000000000000, 0.9238795325112867385, 1.000000000000000000, 0.9238795325112867385, 1.000000000000000000, 0.9238795325112867385, 1.000000000000000000, 0.9238795325112867385, 1.000000000000000000, 0.9238795325112867385, 1.000000000000000000, 0.9238795325112867385, 1.000000000000000000, 0.9238795325112867385, 1.000000000000000000, 0.9238795325112867385, 1.000000000000000000, 0.9238795325112867385, 1.000000000000000000, 0.9238795325112867385, 1.000000000000000000, 0.9238795325112867385, 1.000000000000000000, 0.9238795325112867385, 1.000000000000000000, 0.9238795325112867385, 1.000000000000000000, 0.9238795325112867385, 1.000000000000000000, 0.9238795325112867385, 1.000000000000000000, 0.9238795325112867385, 1.000000000000000000, 0.9238795325112867385, 1.000000000000000000, 0.9238795325112867385, 1.000000000000000000, 0.9238795325112867385, 1.000000000000000000, 0.9238795325112867385, 1.000000000000000000, 0.9238795325112867385, 1.000000000000000000, 0.9238795325112867385, 1.000000000000000000, 0.9238795325112867385, 1.000000000000000000, 0.9238795325112867385, 1.000000000000000000, 0.9238795325112867385, 1.000000000000000000, 0.9238795325112867385, 1.000000000000000000, 0.9238795325112867385, 1.000000000000000000, 0.9238795325112867385, 1.000000000000000000, 0.9238795325112867385, 1.000000000000000000, 0.9238795325112867385, 1.000000000000000000, 0.9238795325112867385, 1.000000000000000000, 0.9238795325112867385, 1.000000000000000000, 0.9238795325112867385, 1.000000000000000000, 0.9238795325112867385, 1.000000000000000000, 0.9238795325112867385, 1.000000000000000000, 0.9238795325112867385, 1.000000000000000000, 0.9238795325112867385, 1.000000000000000000, 0.9238795325112867385, 1.000000000000000000, 0.9238795325112867385, 1.000000000000000000, 0.9238795325112867385, 1.000000000000000000, 0.9238795325112867385, 1.000000000000000000, 0.9238795325112867385, 1.000000000000000000, 0.9238795325112867385, 1.000000000000000000, 0.9238795325112867385, 1.000000000000000000, 0.9238795325112867385, 1.000000000000000000, 0.9238795325112867385, 1.000000000000000000, 0.9238795325112867385, 1.000000000000000000, 0.9238795325112867385, 1.000000000000000000, 0.9238795325112867385, 1.000000000000000000, 0.9238795325112867385, 1.000000000000000000, 0.9238795325112867385, 1.000000000000000000, 0.9238795325112867385, 1.000000000000000000, 0.9238795325112867385, 1.000000000000000000, 0.9238795325112867385, 1.000000000000000000, 0.9238795325112867385, 1.000000000000000000, 0.9238795325112867385, 1.000000000000000000, 0.9238795325112867385, 1.000000000000000000, 0.9238795325112867385, 1.000000000000000000, 0.9238795325112867385, 1.000000000000000000, 0.9238795325112867385, 1.000000000000000000, 0.9238795325112867385, 1.000000000000000000, 0.9238795325112867385, 1.000000000000000000, 0.9238795325112867385, 1.000000000000000000, 0.9238795325112867385, 1.000000000000000000, 0.9238795325112867385, 1.000000000000000000, 0.9238795325112867385, 1.000000000000000000, 0.9238795325112867385, 1.000000000000000000, 0.9238795325112867385, 1.000000000000000000, 0.9238795325112867385, 1.000000000000000000, 0.9238795325112867385, 1.000000000000000000, 0.9238795325112867385, 1.000000000000000000, 0.9238795325112867385, 1.000000000000000000, 0.9238795325112867385, 1.000000000000000000, 0.9238795325112867385, 1.000000000000000000, 0.9238795325112867385, 1.000000000000000000, 0.9238795325112867385, 1.000000000000000000, 0.9238795325112867385, 1.000000000000000000, 0.9238795325112867385, 1.000000000000000000, 0.9238795325112867385, 1.000000000000000000, 0.9238795325112867385, 1.000000000000000000, 0.9238795325112867385, 1.000000000000000000, 0.9238795325112867385, 1.000000000000000000, 0.9238795325112867385, 1.000000000000000000, 0.9238795325112867385, 1.000000000000000000),
 ( 0.3333333333333333703, 0.3079598441704289313, 0.3333333333333333703, 0.3079598441704289313, 0.3333333333333333703, 0.3079598441704289313, 0.3333333333333333703, 0.3079598441704289313, 0.3333333333333333703, 0.3079598441704289313, 0.3333333333333333703, 0.3079598441704289313, 0.3333333333333333703, 0.3079598441704289313, 0.3333333333333333703, 0.3079598441704289313, 0.3333333333333333703, 0.3079598441704289313, 0.3333333333333333703, 0.3079598441704289313, 0.3333333333333333703, 0.3079598441704289313, 0.3333333333333333703, 0.3079598441704289313, 0.3333333333333333703, 0.3079598441704289313, 0.3333333333333333703, 0.3079598441704289313, 0.3333333333333333703, 0.3079598441704289313, 0.3333333333333333703, 0.3079598441704289313, 0.3333333333333333703, 0.3079598441704289313, 0.3333333333333333703, 0.3079598441704289313, 0.3333333333333333703, 0.3079598441704289313, 0.3333333333333333703, 0.3079598441704289313, 0.3333333333333333703, 0.3079598441704289313, 0.3333333333333333703, 0.3079598441704289313, 0.3333333333333333703, 0.3079598441704289313, 0.3333333333333333703, 0.3079598441704289313, 0.3333333333333333703, 0.3079598441704289313, 0.3333333333333333703, 0.3079598441704289313, 0.3333333333333333703, 0.3079598441704289313, 0.3333333333333333703, 0.3079598441704289313, 0.3333333333333333703, 0.3079598441704289313, 0.3333333333333333703, 0.3079598441704289313, 0.3333333333333333703, 0.3079598441704289313, 0.3333333333333333703, 0.3079598441704289313, 0.3333333333333333703, 0.3079598441704289313, 0.3333333333333333703, 0.3079598441704289313, 0.3333333333333333703, 0.3079598441704289313, 0.3333333333333333703, 0.3079598441704289313, 0.3333333333333333703, 0.3079598441704289313, 0.3333333333333333703, 0.3079598441704289313, 0.3333333333333333703, 0.3079598441704289313, 0.3333333333333333703, 0.3079598441704289313, 0.3333333333333333703, 0.3079598441704289313, 0.3333333333333333703, 0.3079598441704289313, 0.3333333333333333703, 0.3079598441704289313, 0.3333333333333333703, 0.3079598441704289313, 0.3333333333333333703, 0.3079598441704289313, 0.3333333333333333703, 0.3079598441704289313, 0.3333333333333333703, 0.3079598441704289313, 0.3333333333333333703, 0.3079598441704289313, 0.3333333333333333703, 0.3079598441704289313, 0.3333333333333333703, 0.3079598441704289313, 0.3333333333333333703, 0.3079598441704289313, 0.3333333333333333703, 0.3079598441704289313, 0.3333333333333333703, 0.3079598441704289313, 0.3333333333333333703, 0.3079598441704289313, 0.3333333333333333703, 0.3079598441704289313, 0.3333333333333333703, 0.3079598441704289313, 0.3333333333333333703, 0.3079598441704289313, 0.3333333333333333703, 0.3079598441704289313, 0.3333333333333333703, 0.3079598441704289313, 0.3333333333333333703, 0.3079598441704289313, 0.3333333333333333703, 0.3079598441704289313, 0.3333333333333333703, 0.3079598441704289313, 0.3333333333333333703, 0.3079598441704289313, 0.3333333333333333703, 0.3079598441704289313, 0.3333333333333333703, 0.3079598441704289313, 0.3333333333333333703, 0.3079598441704289313, 0.3333333333333333703, 0.3079598441704289313, 0.3333333333333333703, 0.3079598441704289313, 0.3333333333333333703, 0.3079598441704289313, 0.3333333333333333703, 0.3079598441704289313, 0.3333333333333333703, 0.3079598441704289313, 0.3333333333333333703, 0.3079598441704289313, 0.3333333333333333703, 0.3079598441704289313, 0.3333333333333333703, 0.3079598441704289313, 0.3333333333333333703, 0.3079598441704289313, 0.3333333333333333703, 0.3079598441704289313, 0.3333333333333333703, 0.3079598441704289313, 0.3333333333333333703, 0.3079598441704289313, 0.3333333333333333703, 0.3079598441704289313, 0.3333333333333333703, 0.3079598441704289313, 0.3333333333333333703, 0.3079598441704289313, 0.3333333333333333703, 0.3079598441704289313, 0.3333333333333333703, 0.3079598441704289313, 0.3333333333333333703, 0.3079598441704289313, 0.3333333333333333703, 0.3079598441704289313, 0.3333333333333333703, 0.3079598441704289313, 0.3333333333333333703, 0.3079598441704289313, 0.3333333333333333703, 0.3079598441704289313, 0.3333333333333333703, 0.3079598441704289313, 0.3333333333333333703, 0.3079598441704289313, 0.3333333333333333703, 0.3079598441704289313, 0.3333333333333333703, 0.3079598441704289313, 0.3333333333333333703, 0.3079598441704289313, 0.3333333333333333703, 0.3079598441704289313, 0.3333333333333333703, 0.3079598441704289313, 0.3333333333333333703, 0.3079598441704289313, 0.3333333333333333703, 0.3079598441704289313, 0.3333333333333333703, 0.3079598441704289313, 0.3333333333333333703, 0.3079598441704289313, 0.3333333333333333703, 0.3079598441704289313, 0.3333333333333333703, 0.3079598441704289313, 0.3333333333333333703, 0.3079598441704289313, 0.3333333333333333703, 0.3079598441704289313, 0.3333333333333333703, 0.3079598441704289313, 0.3333333333333333703, 0.3079598441704289313, 0.3333333333333333703, 0.3079598441704289313, 0.3333333333333333703, 0.3079598441704289313, 0.3333333333333333703, 0.3079598441704289313, 0.3333333333333333703, 0.3079598441704289313, 0.3333333333333333703, 0.3079598441704289313, 0.3333333333333333703, 0.3079598441704289313, 0.3333333333333333703, 0.3079598441704289313, 0.3333333333333333703, 0.3079598441704289313, 0.3333333333333333703, 0.3079598441704289313, 0.3333333333333333703, 0.3079598441704289313, 0.3333333333333333703, 0.3079598441704289313, 0.3333333333333333703, 0.3079598441704289313, 0.3333333333333333703, 0.3079598441704289313, 0.3333333333333333703, 0.3079598441704289313, 0.3333333333333333703, 0.3079598441704289313, 0.3333333333333333703),
 ( 0.3333333333333333703, 0.3079598441704289313, 0.3333333333333333703, 0.3079598441704289313, 0.3333333333333333703, 0.3079598441704289313, 0.3333333333333333703, 0.3079598441704289313, 0.3333333333333333703, 0.3079598441704289313, 0.3333333333333333703, 0.3079598441704289313, 0.3333333333333333703, 0.3079598441704289313, 0.3333333333333333703, 0.3079598441704289313, 0.3333333333333333703, 0.3079598441704289313, 0.3333333333333333703, 0.3079598441704289313, 0.3333333333333333703, 0.3079598441704289313, 0.3333333333333333703, 0.3079598441704289313, 0.3333333333333333703, 0.3079598441704289313, 0.3333333333333333703, 0.3079598441704289313, 0.3333333333333333703, 0.3079598441704289313, 0.3333333333333333703, 0.3079598441704289313, 0.3333333333333333703, 0.3079598441704289313, 0.3333333333333333703, 0.3079598441704289313, 0.3333333333333333703, 0.3079598441704289313, 0.3333333333333333703, 0.3079598441704289313, 0.3333333333333333703, 0.3079598441704289313, 0.3333333333333333703, 0.3079598441704289313, 0.3333333333333333703, 0.3079598441704289313, 0.3333333333333333703, 0.3079598441704289313, 0.3333333333333333703, 0.3079598441704289313, 0.3333333333333333703, 0.3079598441704289313, 0.3333333333333333703, 0.3079598441704289313, 0.3333333333333333703, 0.3079598441704289313, 0.3333333333333333703, 0.3079598441704289313, 0.3333333333333333703, 0.3079598441704289313, 0.3333333333333333703, 0.3079598441704289313, 0.3333333333333333703, 0.3079598441704289313, 0.3333333333333333703, 0.3079598441704289313, 0.3333333333333333703, 0.3079598441704289313, 0.3333333333333333703, 0.3079598441704289313, 0.3333333333333333703, 0.3079598441704289313, 0.3333333333333333703, 0.3079598441704289313, 0.3333333333333333703, 0.3079598441704289313, 0.3333333333333333703, 0.3079598441704289313, 0.3333333333333333703, 0.3079598441704289313, 0.3333333333333333703, 0.3079598441704289313, 0.3333333333333333703, 0.3079598441704289313, 0.3333333333333333703, 0.3079598441704289313, 0.3333333333333333703, 0.3079598441704289313, 0.3333333333333333703, 0.3079598441704289313, 0.3333333333333333703, 0.3079598441704289313, 0.3333333333333333703, 0.3079598441704289313, 0.3333333333333333703, 0.3079598441704289313, 0.3333333333333333703, 0.3079598441704289313, 0.3333333333333333703, 0.3079598441704289313, 0.3333333333333333703, 0.3079598441704289313, 0.3333333333333333703, 0.3079598441704289313, 0.3333333333333333703, 0.3079598441704289313, 0.3333333333333333703, 0.3079598441704289313, 0.3333333333333333703, 0.3079598441704289313, 0.3333333333333333703, 0.3079598441704289313, 0.3333333333333333703, 0.3079598441704289313, 0.3333333333333333703, 0.3079598441704289313, 0.3333333333333333703, 0.3079598441704289313, 0.3333333333333333703, 0.3079598441704289313, 0.3333333333333333703, 0.3079598441704289313, 0.3333333333333333703, 0.3079598441704289313, 0.3333333333333333703, 0.3079598441704289313, 0.3333333333333333703, 0.3079598441704289313, 0.3333333333333333703, 0.3079598441704289313, 0.3333333333333333703, 0.3079598441704289313, 0.3333333333333333703, 0.3079598441704289313, 0.3333333333333333703, 0.3079598441704289313, 0.3333333333333333703, 0.3079598441704289313, 0.3333333333333333703, 0.3079598441704289313, 0.3333333333333333703, 0.3079598441704289313, 0.3333333333333333703, 0.3079598441704289313, 0.3333333333333333703, 0.3079598441704289313, 0.3333333333333333703, 0.3079598441704289313, 0.3333333333333333703, 0.3079598441704289313, 0.3333333333333333703, 0.3079598441704289313, 0.3333333333333333703, 0.3079598441704289313, 0.3333333333333333703, 0.3079598441704289313, 0.3333333333333333703, 0.3079598441704289313, 0.3333333333333333703, 0.3079598441704289313, 0.3333333333333333703, 0.3079598441704289313, 0.3333333333333333703, 0.3079598441704289313, 0.3333333333333333703, 0.3079598441704289313, 0.3333333333333333703, 0.3079598441704289313, 0.3333333333333333703, 0.3079598441704289313, 0.3333333333333333703, 0.3079598441704289313, 0.3333333333333333703, 0.3079598441704289313, 0.3333333333333333703, 0.3079598441704289313, 0.3333333333333333703, 0.3079598441704289313, 0.3333333333333333703, 0.3079598441704289313, 0.3333333333333333703, 0.3079598441704289313, 0.3333333333333333703, 0.3079598441704289313, 0.3333333333333333703, 0.3079598441704289313, 0.3333333333333333703, 0.3079598441704289313, 0.3333333333333333703, 0.3079598441704289313, 0.3333333333333333703, 0.3079598441704289313, 0.3333333333333333703, 0.3079598441704289313, 0.3333333333333333703, 0.3079598441704289313, 0.3333333333333333703, 0.3079598441704289313, 0.3333333333333333703, 0.3079598441704289313, 0.3333333333333333703, 0.3079598441704289313, 0.3333333333333333703, 0.3079598441704289313, 0.3333333333333333703, 0.3079598441704289313, 0.3333333333333333703, 0.3079598441704289313, 0.3333333333333333703, 0.3079598441704289313, 0.3333333333333333703, 0.3079598441704289313, 0.3333333333333333703, 0.3079598441704289313, 0.3333333333333333703, 0.3079598441704289313, 0.3333333333333333703, 0.3079598441704289313, 0.3333333333333333703, 0.3079598441704289313, 0.3333333333333333703, 0.3079598441704289313, 0.3333333333333333703, 0.3079598441704289313, 0.3333333333333333703, 0.3079598441704289313, 0.3333333333333333703, 0.3079598441704289313, 0.3333333333333333703, 0.3079598441704289313, 0.3333333333333333703, 0.3079598441704289313, 0.3333333333333333703, 0.3079598441704289313, 0.3333333333333333703, 0.3079598441704289313, 0.3333333333333333703, 0.3079598441704289313, 0.3333333333333333703, 0.3079598441704289313, 0.3333333333333333703),
 ( 1.000000000000000000, 0.9238795325112867385, 1.000000000000000000, 0.9238795325112867385, 1.000000000000000000, 0.9238795325112867385, 1.000000000000000000, 0.9238795325112867385, 1.000000000000000000, 0.9238795325112867385, 1.000000000000000000, 0.9238795325112867385, 1.000000000000000000, 0.9238795325112867385, 1.000000000000000000, 0.9238795325112867385, 1.000000000000000000, 0.9238795325112867385, 1.000000000000000000, 0.9238795325112867385, 1.000000000000000000, 0.9238795325112867385, 1.000000000000000000, 0.9238795325112867385, 1.000000000000000000, 0.9238795325112867385, 1.000000000000000000, 0.9238795325112867385, 1.000000000000000000, 0.9238795325112867385, 1.000000000000000000, 0.9238795325112867385, 1.000000000000000000, 0.9238795325112867385, 1.000000000000000000, 0.9238795325112867385, 1.000000000000000000, 0.9238795325112867385, 1.000000000000000000, 0.9238795325112867385, 1.000000000000000000, 0.9238795325112867385, 1.000000000000000000, 0.9238795325112867385, 1.000000000000000000, 0.9238795325112867385, 1.000000000000000000, 0.9238795325112867385, 1.000000000000000000, 0.9238795325112867385, 1.000000000000000000, 0.9238795325112867385, 1.000000000000000000, 0.9238795325112867385, 1.000000000000000000, 0.9238795325112867385, 1.000000000000000000, 0.9238795325112867385, 1.000000000000000000, 0.9238795325112867385, 1.000000000000000000, 0.9238795325112867385, 1.000000000000000000, 0.9238795325112867385, 1.000000000000000000, 0.9238795325112867385, 1.000000000000000000, 0.9238795325112867385, 1.000000000000000000, 0.9238795325112867385, 1.000000000000000000, 0.9238795325112867385, 1.000000000000000000, 0.9238795325112867385, 1.000000000000000000, 0.9238795325112867385, 1.000000000000000000, 0.9238795325112867385, 1.000000000000000000, 0.9238795325112867385, 1.000000000000000000, 0.9238795325112867385, 1.000000000000000000, 0.9238795325112867385, 1.000000000000000000, 0.9238795325112867385, 1.000000000000000000, 0.9238795325112867385, 1.000000000000000000, 0.9238795325112867385, 1.000000000000000000, 0.9238795325112867385, 1.000000000000000000, 0.9238795325112867385, 1.000000000000000000, 0.9238795325112867385, 1.000000000000000000, 0.9238795325112867385, 1.000000000000000000, 0.9238795325112867385, 1.000000000000000000, 0.9238795325112867385, 1.000000000000000000, 0.9238795325112867385, 1.000000000000000000, 0.9238795325112867385, 1.000000000000000000, 0.9238795325112867385, 1.000000000000000000, 0.9238795325112867385, 1.000000000000000000, 0.9238795325112867385, 1.000000000000000000, 0.9238795325112867385, 1.000000000000000000, 0.9238795325112867385, 1.000000000000000000, 0.9238795325112867385, 1.000000000000000000, 0.9238795325112867385, 1.000000000000000000, 0.9238795325112867385, 1.000000000000000000, 0.9238795325112867385, 1.000000000000000000, 0.9238795325112867385, 1.000000000000000000, 0.9238795325112867385, 1.000000000000000000, 0.9238795325112867385, 1.000000000000000000, 0.9238795325112867385, 1.000000000000000000, 0.9238795325112867385, 1.000000000000000000, 0.9238795325112867385, 1.000000000000000000, 0.9238795325112867385, 1.000000000000000000, 0.9238795325112867385, 1.000000000000000000, 0.9238795325112867385, 1.000000000000000000, 0.9238795325112867385, 1.000000000000000000, 0.9238795325112867385, 1.000000000000000000, 0.9238795325112867385, 1.000000000000000000, 0.9238795325112867385, 1.000000000000000000, 0.9238795325112867385, 1.000000000000000000, 0.9238795325112867385, 1.000000000000000000, 0.9238795325112867385, 1.000000000000000000, 0.9238795325112867385, 1.000000000000000000, 0.9238795325112867385, 1.000000000000000000, 0.9238795325112867385, 1.000000000000000000, 0.9238795325112867385, 1.000000000000000000, 0.9238795325112867385, 1.000000000000000000, 0.9238795325112867385, 1.000000000000000000, 0.9238795325112867385, 1.000000000000000000, 0.9238795325112867385, 1.000000000000000000, 0.9238795325112867385, 1.000000000000000000, 0.9238795325112867385, 1.000000000000000000, 0.9238795325112867385, 1.000000000000000000, 0.9238795325112867385, 1.000000000000000000, 0.9238795325112867385, 1.000000000000000000, 0.9238795325112867385, 1.000000000000000000, 0.9238795325112867385, 1.000000000000000000, 0.9238795325112867385, 1.000000000000000000, 0.9238795325112867385, 1.000000000000000000, 0.9238795325112867385, 1.000000000000000000, 0.9238795325112867385, 1.000000000000000000, 0.9238795325112867385, 1.000000000000000000, 0.9238795325112867385, 1.000000000000000000, 0.9238795325112867385, 1.000000000000000000, 0.9238795325112867385, 1.000000000000000000, 0.9238795325112867385, 1.000000000000000000, 0.9238795325112867385, 1.000000000000000000, 0.9238795325112867385, 1.000000000000000000, 0.9238795325112867385, 1.000000000000000000, 0.9238795325112867385, 1.000000000000000000, 0.9238795325112867385, 1.000000000000000000, 0.9238795325112867385, 1.000000000000000000, 0.9238795325112867385, 1.000000000000000000, 0.9238795325112867385, 1.000000000000000000, 0.9238795325112867385, 1.000000000000000000, 0.9238795325112867385, 1.000000000000000000, 0.9238795325112867385, 1.000000000000000000, 0.9238795325112867385, 1.000000000000000000, 0.9238795325112867385, 1.000000000000000000, 0.9238795325112867385, 1.000000000000000000, 0.9238795325112867385, 1.000000000000000000, 0.9238795325112867385, 1.000000000000000000, 0.9238795325112867385, 1.000000000000000000, 0.9238795325112867385, 1.000000000000000000),
 ( 0.3333333333333333703, 0.3079598441704289313, 0.3333333333333333703, 0.3079598441704289313, 0.3333333333333333703, 0.3079598441704289313, 0.3333333333333333703, 0.3079598441704289313, 0.3333333333333333703, 0.3079598441704289313, 0.3333333333333333703, 0.3079598441704289313, 0.3333333333333333703, 0.3079598441704289313, 0.3333333333333333703, 0.3079598441704289313, 0.3333333333333333703, 0.3079598441704289313, 0.3333333333333333703, 0.3079598441704289313, 0.3333333333333333703, 0.3079598441704289313, 0.3333333333333333703, 0.3079598441704289313, 0.3333333333333333703, 0.3079598441704289313, 0.3333333333333333703, 0.3079598441704289313, 0.3333333333333333703, 0.3079598441704289313, 0.3333333333333333703, 0.3079598441704289313, 0.3333333333333333703, 0.3079598441704289313, 0.3333333333333333703, 0.3079598441704289313, 0.3333333333333333703, 0.3079598441704289313, 0.3333333333333333703, 0.3079598441704289313, 0.3333333333333333703, 0.3079598441704289313, 0.3333333333333333703, 0.3079598441704289313, 0.3333333333333333703, 0.3079598441704289313, 0.3333333333333333703, 0.3079598441704289313, 0.3333333333333333703, 0.3079598441704289313, 0.3333333333333333703, 0.3079598441704289313, 0.3333333333333333703, 0.3079598441704289313, 0.3333333333333333703, 0.3079598441704289313, 0.3333333333333333703, 0.3079598441704289313, 0.3333333333333333703, 0.3079598441704289313, 0.3333333333333333703, 0.3079598441704289313, 0.3333333333333333703, 0.3079598441704289313, 0.3333333333333333703, 0.3079598441704289313, 0.3333333333333333703, 0.3079598441704289313, 0.3333333333333333703, 0.3079598441704289313, 0.3333333333333333703, 0.3079598441704289313, 0.3333333333333333703, 0.3079598441704289313, 0.3333333333333333703, 0.3079598441704289313, 0.3333333333333333703, 0.3079598441704289313, 0.3333333333333333703, 0.3079598441704289313, 0.3333333333333333703, 0.3079598441704289313, 0.3333333333333333703, 0.3079598441704289313, 0.3333333333333333703, 0.3079598441704289313, 0.3333333333333333703, 0.3079598441704289313, 0.3333333333333333703, 0.3079598441704289313, 0.3333333333333333703, 0.3079598441704289313, 0.3333333333333333703, 0.3079598441704289313, 0.3333333333333333703, 0.3079598441704289313, 0.3333333333333333703, 0.3079598441704289313, 0.3333333333333333703, 0.3079598441704289313, 0.3333333333333333703, 0.3079598441704289313, 0.3333333333333333703, 0.3079598441704289313, 0.3333333333333333703, 0.3079598441704289313, 0.3333333333333333703, 0.3079598441704289313, 0.3333333333333333703, 0.3079598441704289313, 0.3333333333333333703, 0.3079598441704289313, 0.3333333333333333703, 0.3079598441704289313, 0.3333333333333333703, 0.3079598441704289313, 0.3333333333333333703, 0.3079598441704289313, 0.3333333333333333703, 0.3079598441704289313, 0.3333333333333333703, 0.3079598441704289313, 0.3333333333333333703, 0.3079598441704289313, 0.3333333333333333703, 0.3079598441704289313, 0.3333333333333333703, 0.3079598441704289313, 0.3333333333333333703, 0.3079598441704289313, 0.3333333333333333703, 0.3079598441704289313, 0.3333333333333333703, 0.3079598441704289313, 0.3333333333333333703, 0.3079598441704289313, 0.3333333333333333703, 0.3079598441704289313, 0.3333333333333333703, 0.3079598441704289313, 0.3333333333333333703, 0.3079598441704289313, 0.3333333333333333703, 0.3079598441704289313, 0.3333333333333333703, 0.3079598441704289313, 0.3333333333333333703, 0.3079598441704289313, 0.3333333333333333703, 0.3079598441704289313, 0.3333333333333333703, 0.3079598441704289313, 0.3333333333333333703, 0.3079598441704289313, 0.3333333333333333703, 0.3079598441704289313, 0.3333333333333333703, 0.3079598441704289313, 0.3333333333333333703, 0.3079598441704289313, 0.3333333333333333703, 0.3079598441704289313, 0.3333333333333333703, 0.3079598441704289313, 0.3333333333333333703, 0.3079598441704289313, 0.3333333333333333703, 0.3079598441704289313, 0.3333333333333333703, 0.3079598441704289313, 0.3333333333333333703, 0.3079598441704289313, 0.3333333333333333703, 0.3079598441704289313, 0.3333333333333333703, 0.3079598441704289313, 0.3333333333333333703, 0.3079598441704289313, 0.3333333333333333703, 0.3079598441704289313, 0.3333333333333333703, 0.3079598441704289313, 0.3333333333333333703, 0.3079598441704289313, 0.3333333333333333703, 0.3079598441704289313, 0.3333333333333333703, 0.3079598441704289313, 0.3333333333333333703, 0.3079598441704289313, 0.3333333333333333703, 0.3079598441704289313, 0.3333333333333333703, 0.3079598441704289313, 0.3333333333333333703, 0.3079598441704289313, 0.3333333333333333703, 0.3079598441704289313, 0.3333333333333333703, 0.3079598441704289313, 0.3333333333333333703, 0.3079598441704289313, 0.3333333333333333703, 0.3079598441704289313, 0.3333333333333333703, 0.3079598441704289313, 0.3333333333333333703, 0.3079598441704289313, 0.3333333333333333703, 0.3079598441704289313, 0.3333333333333333703, 0.3079598441704289313, 0.3333333333333333703, 0.3079598441704289313, 0.3333333333333333703, 0.3079598441704289313, 0.3333333333333333703, 0.3079598441704289313, 0.3333333333333333703, 0.3079598441704289313, 0.3333333333333333703, 0.3079598441704289313, 0.3333333333333333703, 0.3079598441704289313, 0.3333333333333333703, 0.3079598441704289313, 0.3333333333333333703, 0.3079598441704289313, 0.3333333333333333703, 0.3079598441704289313, 0.3333333333333333703, 0.3079598441704289313, 0.3333333333333333703, 0.3079598441704289313, 0.3333333333333333703, 0.3079598441704289313, 0.3333333333333333703, 0.3079598441704289313, 0.3333333333333333703, 0.3079598441704289313, 0.3333333333333333703),
 ( 0.3333333333333333703, 0.3079598441704289313, 0.3333333333333333703, 0.3079598441704289313, 0.3333333333333333703, 0.3079598441704289313, 0.3333333333333333703, 0.3079598441704289313, 0.3333333333333333703, 0.3079598441704289313, 0.3333333333333333703, 0.3079598441704289313, 0.3333333333333333703, 0.3079598441704289313, 0.3333333333333333703, 0.3079598441704289313, 0.3333333333333333703, 0.3079598441704289313, 0.3333333333333333703, 0.3079598441704289313, 0.3333333333333333703, 0.3079598441704289313, 0.3333333333333333703, 0.3079598441704289313, 0.3333333333333333703, 0.3079598441704289313, 0.3333333333333333703, 0.3079598441704289313, 0.3333333333333333703, 0.3079598441704289313, 0.3333333333333333703, 0.3079598441704289313, 0.3333333333333333703, 0.3079598441704289313, 0.3333333333333333703, 0.3079598441704289313, 0.3333333333333333703, 0.3079598441704289313, 0.3333333333333333703, 0.3079598441704289313, 0.3333333333333333703, 0.3079598441704289313, 0.3333333333333333703, 0.3079598441704289313, 0.3333333333333333703, 0.3079598441704289313, 0.3333333333333333703, 0.3079598441704289313, 0.3333333333333333703, 0.3079598441704289313, 0.3333333333333333703, 0.3079598441704289313, 0.3333333333333333703, 0.3079598441704289313, 0.3333333333333333703, 0.3079598441704289313, 0.3333333333333333703, 0.3079598441704289313, 0.3333333333333333703, 0.3079598441704289313, 0.3333333333333333703, 0.3079598441704289313, 0.3333333333333333703, 0.3079598441704289313, 0.3333333333333333703, 0.3079598441704289313, 0.3333333333333333703, 0.3079598441704289313, 0.3333333333333333703, 0.3079598441704289313, 0.3333333333333333703, 0.3079598441704289313, 0.3333333333333333703, 0.3079598441704289313, 0.3333333333333333703, 0.3079598441704289313, 0.3333333333333333703, 0.3079598441704289313, 0.3333333333333333703, 0.3079598441704289313, 0.3333333333333333703, 0.3079598441704289313, 0.3333333333333333703, 0.3079598441704289313, 0.3333333333333333703, 0.3079598441704289313, 0.3333333333333333703, 0.3079598441704289313, 0.3333333333333333703, 0.3079598441704289313, 0.3333333333333333703, 0.3079598441704289313, 0.3333333333333333703, 0.3079598441704289313, 0.3333333333333333703, 0.3079598441704289313, 0.3333333333333333703, 0.3079598441704289313, 0.3333333333333333703, 0.3079598441704289313, 0.3333333333333333703, 0.3079598441704289313, 0.3333333333333333703, 0.3079598441704289313, 0.3333333333333333703, 0.3079598441704289313, 0.3333333333333333703, 0.3079598441704289313, 0.3333333333333333703, 0.3079598441704289313, 0.3333333333333333703, 0.3079598441704289313, 0.3333333333333333703, 0.3079598441704289313, 0.3333333333333333703, 0.3079598441704289313, 0.3333333333333333703, 0.3079598441704289313, 0.3333333333333333703, 0.3079598441704289313, 0.3333333333333333703, 0.3079598441704289313, 0.3333333333333333703, 0.3079598441704289313, 0.3333333333333333703, 0.3079598441704289313, 0.3333333333333333703, 0.3079598441704289313, 0.3333333333333333703, 0.3079598441704289313, 0.3333333333333333703, 0.3079598441704289313, 0.3333333333333333703, 0.3079598441704289313, 0.3333333333333333703, 0.3079598441704289313, 0.3333333333333333703, 0.3079598441704289313, 0.3333333333333333703, 0.3079598441704289313, 0.3333333333333333703, 0.3079598441704289313, 0.3333333333333333703, 0.3079598441704289313, 0.3333333333333333703, 0.3079598441704289313, 0.3333333333333333703, 0.3079598441704289313, 0.3333333333333333703, 0.3079598441704289313, 0.3333333333333333703, 0.3079598441704289313, 0.3333333333333333703, 0.3079598441704289313, 0.3333333333333333703, 0.3079598441704289313, 0.3333333333333333703, 0.3079598441704289313, 0.3333333333333333703, 0.3079598441704289313, 0.3333333333333333703, 0.3079598441704289313, 0.3333333333333333703, 0.3079598441704289313, 0.3333333333333333703, 0.3079598441704289313, 0.3333333333333333703, 0.3079598441704289313, 0.3333333333333333703, 0.3079598441704289313, 0.3333333333333333703, 0.3079598441704289313, 0.3333333333333333703, 0.3079598441704289313, 0.3333333333333333703, 0.3079598441704289313, 0.3333333333333333703, 0.3079598441704289313, 0.3333333333333333703, 0.3079598441704289313, 0.3333333333333333703, 0.3079598441704289313, 0.3333333333333333703, 0.3079598441704289313, 0.3333333333333333703, 0.3079598441704289313, 0.3333333333333333703, 0.3079598441704289313, 0.3333333333333333703, 0.3079598441704289313, 0.3333333333333333703, 0.3079598441704289313, 0.3333333333333333703, 0.3079598441704289313, 0.3333333333333333703, 0.3079598441704289313, 0.3333333333333333703, 0.3079598441704289313, 0.3333333333333333703, 0.3079598441704289313, 0.3333333333333333703, 0.3079598441704289313, 0.3333333333333333703, 0.3079598441704289313, 0.3333333333333333703, 0.3079598441704289313, 0.3333333333333333703, 0.3079598441704289313, 0.3333333333333333703, 0.3079598441704289313, 0.3333333333333333703, 0.3079598441704289313, 0.3333333333333333703, 0.3079598441704289313, 0.3333333333333333703, 0.3079598441704289313, 0.3333333333333333703, 0.3079598441704289313, 0.3333333333333333703, 0.3079598441704289313, 0.3333333333333333703, 0.3079598441704289313, 0.3333333333333333703, 0.3079598441704289313, 0.3333333333333333703, 0.3079598441704289313, 0.3333333333333333703, 0.3079598441704289313, 0.3333333333333333703, 0.3079598441704289313, 0.3333333333333333703, 0.3079598441704289313, 0.3333333333333333703, 0.3079598441704289313, 0.3333333333333333703, 0.3079598441704289313, 0.3333333333333333703, 0.3079598441704289313, 0.3333333333333333703, 0.3079598441704289313, 0.3333333333333333703),
 ( 1.000000000000000000, 0.9238795325112867385, 1.000000000000000000, 0.9238795325112867385, 1.000000000000000000, 0.9238795325112867385, 1.000000000000000000, 0.9238795325112867385, 1.000000000000000000, 0.9238795325112867385, 1.000000000000000000, 0.9238795325112867385, 1.000000000000000000, 0.9238795325112867385, 1.000000000000000000, 0.9238795325112867385, 1.000000000000000000, 0.9238795325112867385, 1.000000000000000000, 0.9238795325112867385, 1.000000000000000000, 0.9238795325112867385, 1.000000000000000000, 0.9238795325112867385, 1.000000000000000000, 0.9238795325112867385, 1.000000000000000000, 0.9238795325112867385, 1.000000000000000000, 0.9238795325112867385, 1.000000000000000000, 0.9238795325112867385, 1.000000000000000000, 0.9238795325112867385, 1.000000000000000000, 0.9238795325112867385, 1.000000000000000000, 0.9238795325112867385, 1.000000000000000000, 0.9238795325112867385, 1.000000000000000000, 0.9238795325112867385, 1.000000000000000000, 0.9238795325112867385, 1.000000000000000000, 0.9238795325112867385, 1.000000000000000000, 0.9238795325112867385, 1.000000000000000000, 0.9238795325112867385, 1.000000000000000000, 0.9238795325112867385, 1.000000000000000000, 0.9238795325112867385, 1.000000000000000000, 0.9238795325112867385, 1.000000000000000000, 0.9238795325112867385, 1.000000000000000000, 0.9238795325112867385, 1.000000000000000000, 0.9238795325112867385, 1.000000000000000000, 0.9238795325112867385, 1.000000000000000000, 0.9238795325112867385, 1.000000000000000000, 0.9238795325112867385, 1.000000000000000000, 0.9238795325112867385, 1.000000000000000000, 0.9238795325112867385, 1.000000000000000000, 0.9238795325112867385, 1.000000000000000000, 0.9238795325112867385, 1.000000000000000000, 0.9238795325112867385, 1.000000000000000000, 0.9238795325112867385, 1.000000000000000000, 0.9238795325112867385, 1.000000000000000000, 0.9238795325112867385, 1.000000000000000000, 0.9238795325112867385, 1.000000000000000000, 0.9238795325112867385, 1.000000000000000000, 0.9238795325112867385, 1.000000000000000000, 0.9238795325112867385, 1.000000000000000000, 0.9238795325112867385, 1.000000000000000000, 0.9238795325112867385, 1.000000000000000000, 0.9238795325112867385, 1.000000000000000000, 0.9238795325112867385, 1.000000000000000000, 0.9238795325112867385, 1.000000000000000000, 0.9238795325112867385, 1.000000000000000000, 0.9238795325112867385, 1.000000000000000000, 0.9238795325112867385, 1.000000000000000000, 0.9238795325112867385, 1.000000000000000000, 0.9238795325112867385, 1.000000000000000000, 0.9238795325112867385, 1.000000000000000000, 0.9238795325112867385, 1.000000000000000000, 0.9238795325112867385, 1.000000000000000000, 0.9238795325112867385, 1.000000000000000000, 0.9238795325112867385, 1.000000000000000000, 0.9238795325112867385, 1.000000000000000000, 0.9238795325112867385, 1.000000000000000000, 0.9238795325112867385, 1.000000000000000000, 0.9238795325112867385, 1.000000000000000000, 0.9238795325112867385, 1.000000000000000000, 0.9238795325112867385, 1.000000000000000000, 0.9238795325112867385, 1.000000000000000000, 0.9238795325112867385, 1.000000000000000000, 0.9238795325112867385, 1.000000000000000000, 0.9238795325112867385, 1.000000000000000000, 0.9238795325112867385, 1.000000000000000000, 0.9238795325112867385, 1.000000000000000000, 0.9238795325112867385, 1.000000000000000000, 0.9238795325112867385, 1.000000000000000000, 0.9238795325112867385, 1.000000000000000000, 0.9238795325112867385, 1.000000000000000000, 0.9238795325112867385, 1.000000000000000000, 0.9238795325112867385, 1.000000000000000000, 0.9238795325112867385, 1.000000000000000000, 0.9238795325112867385, 1.000000000000000000, 0.9238795325112867385, 1.000000000000000000, 0.9238795325112867385, 1.000000000000000000, 0.9238795325112867385, 1.000000000000000000, 0.9238795325112867385, 1.000000000000000000, 0.9238795325112867385, 1.000000000000000000, 0.9238795325112867385, 1.000000000000000000, 0.9238795325112867385, 1.000000000000000000, 0.9238795325112867385, 1.000000000000000000, 0.9238795325112867385, 1.000000000000000000, 0.9238795325112867385, 1.000000000000000000, 0.9238795325112867385, 1.000000000000000000, 0.9238795325112867385, 1.000000000000000000, 0.9238795325112867385, 1.000000000000000000, 0.9238795325112867385, 1.000000000000000000, 0.9238795325112867385, 1.000000000000000000, 0.9238795325112867385, 1.000000000000000000, 0.9238795325112867385, 1.000000000000000000, 0.9238795325112867385, 1.000000000000000000, 0.9238795325112867385, 1.000000000000000000, 0.9238795325112867385, 1.000000000000000000, 0.9238795325112867385, 1.000000000000000000, 0.9238795325112867385, 1.000000000000000000, 0.9238795325112867385, 1.000000000000000000, 0.9238795325112867385, 1.000000000000000000, 0.9238795325112867385, 1.000000000000000000, 0.9238795325112867385, 1.000000000000000000, 0.9238795325112867385, 1.000000000000000000, 0.9238795325112867385, 1.000000000000000000, 0.9238795325112867385, 1.000000000000000000, 0.9238795325112867385, 1.000000000000000000, 0.9238795325112867385, 1.000000000000000000, 0.9238795325112867385, 1.000000000000000000, 0.9238795325112867385, 1.000000000000000000, 0.9238795325112867385, 1.000000000000000000, 0.9238795325112867385, 1.000000000000000000, 0.9238795325112867385, 1.000000000000000000, 0.9238795325112867385, 1.000000000000000000, 0.9238795325112867385, 1.000000000000000000, 0.9238795325112867385, 1.000000000000000000) ) ) 
 REPRESENTATION_ITEM ( '' )  SURFACE ( )  );
#6559 = CARTESIAN_POINT ( 'NONE',  ( 10.93719894220377320, 13.85079060082045466, -106.6657003074759587 ) ) ;
#6560 = CARTESIAN_POINT ( 'NONE',  ( 1.346194077712560944, 6.937500000000000000, -0.2500000000000010547 ) ) ;
#6561 = CARTESIAN_POINT ( 'NONE',  ( -3.750000000000000000, 5.812500000000000888, -5.053300858899105741 ) ) ;
#6562 = CARTESIAN_POINT ( 'NONE',  ( 3.749999999999999556, 9.812500000000000000, -1.946699141100892261 ) ) ;
#6563 = ADVANCED_FACE ( 'NONE', ( #2231 ), #1147, .T. ) ;
#6564 = CARTESIAN_POINT ( 'NONE',  ( -13.42077998717343057, 7.499999999999991118, -89.47651029354803143 ) ) ;
#6565 = ORIENTED_EDGE ( 'NONE', *, *, #10523, .F. ) ;
#6566 = CARTESIAN_POINT ( 'NONE',  ( -3.782526895735886630, 9.999999999999996447, -42.84475209785864536 ) ) ;
#6567 = CARTESIAN_POINT ( 'NONE',  ( 0.000000000000000000, 11.50000000000000000, 0.2500000000000002220 ) ) ;
#6568 = CARTESIAN_POINT ( 'NONE',  ( 1.114947364559093712, 6.000000000000000000, -139.4079432275550232 ) ) ;
#6569 = CARTESIAN_POINT ( 'NONE',  ( 0.000000000000000000, 1.000000000000000000, 0.000000000000000000 ) ) ;
#6570 = CARTESIAN_POINT ( 'NONE',  ( 7.427446726622314976, 7.321094445766561876, -26.41501464507892294 ) ) ;
#6571 = ORIENTED_EDGE ( 'NONE', *, *, #2786, .T. ) ;
#6572 = CARTESIAN_POINT ( 'NONE',  ( -17.92852900003595806, 3.999999999999993783, -157.6654428080335890 ) ) ;
#6573 = CARTESIAN_POINT ( 'NONE',  ( 1.346194077712560944, 0.9375000000000000000, -0.2500000000000011102 ) ) ;
#6574 = CARTESIAN_POINT ( 'NONE',  ( -30.85915506344845483, 9.999999999999998224, -156.4241655052078954 ) ) ;
#6575 = CARTESIAN_POINT ( 'NONE',  ( -3.980102097228897738E-16, 1.084202172485504434E-16, -6.749999999999999112 ) ) ;
#6576 = EDGE_LOOP ( 'NONE', ( #13071, #111, #4168, #8513 ) ) ;
#6577 = DIRECTION ( 'NONE',  ( -0.02058562339462809143, 0.3314513491899346298, 0.9432477061883728364 ) ) ;
#6578 = CARTESIAN_POINT ( 'NONE',  ( 11.32016196459912649, 5.000000000000000888, -106.4092894470390291 ) ) ;
#6579 = CYLINDRICAL_SURFACE ( 'NONE', #10218, 16.00000000006737721 ) ;
#6580 = CARTESIAN_POINT ( 'NONE',  ( -3.249999999999999556, 10.25000000000000000, -3.499999999999999556 ) ) ;
#6581 = CARTESIAN_POINT ( 'NONE',  ( -6.992168204689655830, 14.99999999999999645, -113.2636094677312855 ) ) ;
#6582 = CARTESIAN_POINT ( 'NONE',  ( -9.385448347264278013, 5.000000000000000888, -115.3551636530117293 ) ) ;
#6583 = CARTESIAN_POINT ( 'NONE',  ( 1.346194077712561166, 9.437500000000003553, -0.2500000000000011102 ) ) ;
#6584 = EDGE_CURVE ( 'NONE', #9158, #914, #15237, .T. ) ;
#6585 = LINE ( 'NONE', #10139, #2997 ) ;
#6586 = CARTESIAN_POINT ( 'NONE',  ( -2.651650429449553314, 14.37500000000000000, -6.151650429449552426 ) ) ;
#6587 = CARTESIAN_POINT ( 'NONE',  ( -18.09353981420494151, 5.000000000000000000, -129.3374956033359240 ) ) ;
#6588 = ADVANCED_FACE ( 'NONE', ( #10569, #6938 ), #3462, .T. ) ;
#6589 = EDGE_CURVE ( 'NONE', #9845, #12491, #596, .T. ) ;
#6590 = DIRECTION ( 'NONE',  ( 0.000000000000000000, -1.000000000000000000, 0.000000000000000000 ) ) ;
#6591 = CARTESIAN_POINT ( 'NONE',  ( -3.249999999999999556, 10.18750000000000000, -2.153805922287440833 ) ) ;
#6592 = CARTESIAN_POINT ( 'NONE',  ( -9.306320601523868419, 2.743867526398027223, -40.23124431751398333 ) ) ;
#6593 = CIRCLE ( 'NONE', #8553, 0.5000000000000004441 ) ;
#6594 = LINE ( 'NONE', #11382, #9481 ) ;
#6595 = CARTESIAN_POINT ( 'NONE',  ( -3.249999999999999556, 8.312500000000000000, -4.846194077712557835 ) ) ;
#6596 = CARTESIAN_POINT ( 'NONE',  ( -1.141970775756692369, 8.673617379884035472E-16, -133.1539114526842695 ) ) ;
#6597 = CARTESIAN_POINT ( 'NONE',  ( 0.4616602863826347325, 7.217962787865914056E-16, -0.1920150514337511105 ) ) ;
#6598 = ORIENTED_EDGE ( 'NONE', *, *, #5263, .F. ) ;
#6599 = CARTESIAN_POINT ( 'NONE',  ( 9.943023108890812978, 5.000000000000002665, -43.30782091980648829 ) ) ;
#6600 = CARTESIAN_POINT ( 'NONE',  ( -4.507463604512252253, 5.000000000000000000, -2.585105772303598393 ) ) ;
#6601 = CARTESIAN_POINT ( 'NONE',  ( -4.592425496802573972E-16, 0.5000000000000000000, -7.249999999999999112 ) ) ;
#6602 = CARTESIAN_POINT ( 'NONE',  ( -1.553300858899106629, 0.5625000000000001110, 0.2499999999999998335 ) ) ;
#6603 = CARTESIAN_POINT ( 'NONE',  ( -1.346194077712559389, 0.4375000000000000555, -6.749999999999999112 ) ) ;
#6604 = ORIENTED_EDGE ( 'NONE', *, *, #438, .F. ) ;
#6605 = CIRCLE ( 'NONE', #9316, 0.9999999999999988898 ) ;
#6606 = CARTESIAN_POINT ( 'NONE',  ( -2.298097038856278473, 10.12500000000000000, -1.201902961143720416 ) ) ;
#6607 = B_SPLINE_CURVE_WITH_KNOTS ( 'NONE', 3,
 ( #4535, #4382, #12569, #1835, #12729, #679, #11331, #4456, #5462, #5534, #9090, #9015, #9247, #13972, #10254, #7700, #7852, #5384 ),
 .UNSPECIFIED., .F., .F.,
 ( 4, 2, 2, 2, 2, 2, 2, 2, 4 ),
 ( 1.734723475976807094E-18, 0.001049529208182716509, 0.002099058416365431282, 0.003148587624548146273, 0.004198116832730860830, 0.005247646040913573652, 0.006297175249096287342, 0.007346704457279000164, 0.008396233665461712986 ),
 .UNSPECIFIED. ) ;
#6608 = CARTESIAN_POINT ( 'NONE',  ( 9.991047690016531035, 12.61351667247251740, -45.61670005978161413 ) ) ;
#6609 = EDGE_CURVE ( 'NONE', #3281, #11204, #5850, .T. ) ;
#6610 = APPLICATION_CONTEXT ( 'configuration controlled 3d designs of mechanical parts and assemblies' ) ;
#6611 = CARTESIAN_POINT ( 'NONE',  ( 13.58051105728158880, 13.61566402447629365, -126.1567731084821702 ) ) ;
#6612 = CARTESIAN_POINT ( 'NONE',  ( 7.788671722263534214, 5.321094445766561876, -20.36947622874119546 ) ) ;
#6613 = CARTESIAN_POINT ( 'NONE',  ( -9.868623142304215889, 10.39218436379010591, -115.7530035197778631 ) ) ;
#6614 = PERSON_AND_ORGANIZATION_ROLE ( 'creator' ) ;
#6615 = CARTESIAN_POINT ( 'NONE',  ( 8.459890227587649747, 14.99999999999906386, -115.7934283673361477 ) ) ;
#6616 = CARTESIAN_POINT ( 'NONE',  ( -7.749031843371196437, 13.85782642611278170, -116.8124745394366641 ) ) ;
#6617 = CARTESIAN_POINT ( 'NONE',  ( 3.158384440324536691, 0.000000000000000000, -1.000000000000001332 ) ) ;
#6618 = VERTEX_POINT ( 'NONE', #4400 ) ;
#6619 = CARTESIAN_POINT ( 'NONE',  ( -3.249999999999999556, 4.187500000000000000, -2.153805922287440833 ) ) ;
#6620 = FACE_OUTER_BOUND ( 'NONE', #1442, .T. ) ;
#6621 = CARTESIAN_POINT ( 'NONE',  ( -3.750000000000000000, 1.687500000000000222, -1.946699141100893149 ) ) ;
#6622 = ORIENTED_EDGE ( 'NONE', *, *, #14045, .F. ) ;
#6623 = CARTESIAN_POINT ( 'NONE',  ( -4.234402844927150689, 0.000000000000000000, -117.4888040839639558 ) ) ;
#6624 = FACE_OUTER_BOUND ( 'NONE', #13810, .T. ) ;
#6625 = CARTESIAN_POINT ( 'NONE',  ( 3.749999999999998668, 6.687500000000000888, -5.053300858899107517 ) ) ;
#6626 = CARTESIAN_POINT ( 'NONE',  ( -63.21422130130007133, 10.00000000000000178, -203.6040552426024988 ) ) ;
#6627 = CARTESIAN_POINT ( 'NONE',  ( 2.998665091981967734, 1.009082376855201968, 3.243864481526151256 ) ) ;
#6628 = CARTESIAN_POINT ( 'NONE',  ( -2.651650429449552870, 2.125000000000000000, -0.8483495705504462414 ) ) ;
#6629 = CALENDAR_DATE ( 2026, 8, 10 ) ;
#6630 = CARTESIAN_POINT ( 'NONE',  ( 20.29380258822241956, 5.000000000000000888, -132.2785196063218223 ) ) ;
#6631 = VERTEX_POINT ( 'NONE', #14139 ) ;
#6632 = CARTESIAN_POINT ( 'NONE',  ( -35.09122780324831581, 15.00000000000000178, -151.1986770539716076 ) ) ;
#6633 = CARTESIAN_POINT ( 'NONE',  ( 1.346194077712561166, 4.437499999999999112, -0.2500000000000011102 ) ) ;
#6634 = CARTESIAN_POINT ( 'NONE',  ( 26.28048204801264731, 0.000000000000000000, 69.48733826436532013 ) ) ;
#6635 = CIRCLE ( 'NONE', #15051, 2.250000000000005773 ) ;
#6636 = CARTESIAN_POINT ( 'NONE',  ( -8.645680077366938221, 4.728706406862280561E-12, -122.8677831019022619 ) ) ;
#6637 = CARTESIAN_POINT ( 'NONE',  ( -4.592425496802573972E-16, 5.999999999999999112, -7.250000000000000000 ) ) ;
#6638 = CARTESIAN_POINT ( 'NONE',  ( 2.651650429449552870, 9.625000000000000000, -6.151650429449554203 ) ) ;
#6639 = CARTESIAN_POINT ( 'NONE',  ( -7.289398910521280861, 0.9469664532186193862, -116.2745874757426776 ) ) ;
#6640 = VERTEX_POINT ( 'NONE', #10271 ) ;
#6641 = CARTESIAN_POINT ( 'NONE',  ( 0.4711736884522539359, 9.999999999999998224, 5.336993082470237404 ) ) ;
#6642 = CARTESIAN_POINT ( 'NONE',  ( 2.651650429449552870, 12.12500000000000000, -6.151650429449555091 ) ) ;
#6643 = DIRECTION ( 'NONE',  ( 0.000000000000000000, -0.000000000000000000, 1.000000000000000000 ) ) ;
#6644 = CARTESIAN_POINT ( 'NONE',  ( 0.4616602863826355096, 0.000000000000000000, -0.1920150514337429226 ) ) ;
#6645 = VERTEX_POINT ( 'NONE', #6796 ) ;
#6646 = CARTESIAN_POINT ( 'NONE',  ( -12.67859807986386400, 2.739772825377753718E-13, -152.4516537531287099 ) ) ;
#6647 = FACE_OUTER_BOUND ( 'NONE', #8347, .T. ) ;
#6648 =( BOUNDED_SURFACE ( )  B_SPLINE_SURFACE ( 3, 2, ( 
 ( #1554, #13310, #7177 ),
 ( #3639, #3796, #6105 ),
 ( #400, #9584, #8501 ),
 ( #14480, #14310, #9824 ),
 ( #8341, #2482, #14556 ),
 ( #10983, #8659, #13392 ),
 ( #13236, #8420, #2637 ),
 ( #12053, #11058, #321 ),
 ( #7499, #12219, #475 ),
 ( #11900, #7651, #12367 ),
 ( #10125, #6646, #10051 ),
 ( #13544, #7874, #2874 ),
 ( #6572, #6496, #8965 ),
 ( #7573, #1935, #553 ),
 ( #10208, #11284, #11356 ),
 ( #5265, #14790, #11213 ),
 ( #12292, #2943, #632 ),
 ( #705, #1785, #1702 ),
 ( #5411, #9975, #7807 ),
 ( #6416, #12447, #4184 ),
 ( #784, #5489, #8890 ),
 ( #9043, #13766, #14867 ),
 ( #5337, #859, #11135 ),
 ( #13622, #3023, #7730 ),
 ( #14714, #1867, #3161 ),
 ( #4263, #12595, #11437 ),
 ( #13695, #14942, #8815 ),
 ( #14638, #3093, #12519 ),
 ( #6724, #2014, #5561 ),
 ( #4035, #4337, #8740 ),
 ( #13471, #4113, #10507 ),
 ( #1080, #3392, #2166 ),
 ( #11514, #12673, #5855 ),
 ( #7018, #12827, #929 ),
 ( #6868, #2237, #7953 ),
 ( #11582, #2088, #6945 ),
 ( #3240, #10347, #11661 ),
 ( #9190, #2386, #13838 ),
 ( #15241, #6799, #14145 ),
 ( #10276, #15313, #4708 ),
 ( #5786, #10574, #1152 ),
 ( #5631, #9112, #12981 ) ),
 .UNSPECIFIED., .F., .F., .T. ) 
 B_SPLINE_SURFACE_WITH_KNOTS ( ( 4, 2, 2, 2, 2, 2, 2, 2, 2, 2, 2, 2, 2, 2, 2, 2, 2, 2, 2, 2, 4 ),
 ( 3, 3 ),
 ( 0.09990852050945690788, 0.1044989422773630605, 0.1090893640452691993, 0.1136797858131753519, 0.1159749966971284352, 0.1182702075810815046, 0.1274510511168938098, 0.1366318946527061151, 0.1412223164206122816, 0.1435175273045653510, 0.1458127381885184204, 0.1504031599564245592, 0.1549935817243306979, 0.1595840034922368367, 0.1618792143761899061, 0.1641744252601430032, 0.1664696361440961003, 0.1687648470280491697, 0.1699124524700257044, 0.1710600579120022391, 0.1733552687959553085 ),
 ( 0.1371266450457513664, 1.000000000000000000 ),
 .UNSPECIFIED. ) 
 GEOMETRIC_REPRESENTATION_ITEM ( )  RATIONAL_B_SPLINE_SURFACE ( (
 ( 0.9306880333625024981, 0.7472702456390873937, 1.000000000000000000),
 ( 0.9306880333625024981, 0.7472702456390873937, 1.000000000000000000),
 ( 0.9306880333625024981, 0.7472702456390873937, 1.000000000000000000),
 ( 0.9306880333625024981, 0.7472702456390873937, 1.000000000000000000),
 ( 0.9306880333625024981, 0.7472702456390873937, 1.000000000000000000),
 ( 0.9306880333625024981, 0.7472702456390873937, 1.000000000000000000),
 ( 0.9306880333625024981, 0.7472702456390873937, 1.000000000000000000),
 ( 0.9306880333625024981, 0.7472702456390873937, 1.000000000000000000),
 ( 0.9306880333625024981, 0.7472702456390873937, 1.000000000000000000),
 ( 0.9306880333625024981, 0.7472702456390873937, 1.000000000000000000),
 ( 0.9306880333625024981, 0.7472702456390873937, 1.000000000000000000),
 ( 0.9306880333625024981, 0.7472702456390873937, 1.000000000000000000),
 ( 0.9306880333625024981, 0.7472702456390875048, 1.000000000000000000),
 ( 0.9306880333625024981, 0.7472702456390875048, 1.000000000000000000),
 ( 0.9306880333625024981, 0.7472702456390873937, 1.000000000000000000),
 ( 0.9306880333625024981, 0.7472702456390873937, 1.000000000000000000),
 ( 0.9306880333625022761, 0.7472702456390867276, 1.000000000000000000),
 ( 0.9306880333625022761, 0.7472702456390867276, 1.000000000000000000),
 ( 0.9306880333625024981, 0.7472702456390873937, 1.000000000000000000),
 ( 0.9306880333625024981, 0.7472702456390873937, 1.000000000000000000),
 ( 0.9306880333625022761, 0.7472702456390867276, 1.000000000000000000),
 ( 0.9306880333625022761, 0.7472702456390867276, 1.000000000000000000),
 ( 0.9306880333625024981, 0.7472702456390873937, 1.000000000000000000),
 ( 0.9306880333625024981, 0.7472702456390873937, 1.000000000000000000),
 ( 0.9306880333625024981, 0.7472702456390876158, 1.000000000000000000),
 ( 0.9306880333625024981, 0.7472702456390876158, 1.000000000000000000),
 ( 0.9306880333625024981, 0.7472702456390873937, 1.000000000000000000),
 ( 0.9306880333625024981, 0.7472702456390873937, 1.000000000000000000),
 ( 0.9306880333625024981, 0.7472702456390873937, 1.000000000000000000),
 ( 0.9306880333625024981, 0.7472702456390873937, 1.000000000000000000),
 ( 0.9306880333625024981, 0.7472702456390873937, 1.000000000000000000),
 ( 0.9306880333625024981, 0.7472702456390873937, 1.000000000000000000),
 ( 0.9306880333625024981, 0.7472702456390873937, 1.000000000000000000),
 ( 0.9306880333625024981, 0.7472702456390873937, 1.000000000000000000),
 ( 0.9306880333625024981, 0.7472702456390873937, 1.000000000000000000),
 ( 0.9306880333625024981, 0.7472702456390873937, 1.000000000000000000),
 ( 0.9306880333625024981, 0.7472702456390873937, 1.000000000000000000),
 ( 0.9306880333625024981, 0.7472702456390873937, 1.000000000000000000),
 ( 0.9306880333625024981, 0.7472702456390875048, 1.000000000000000000),
 ( 0.9306880333625024981, 0.7472702456390875048, 1.000000000000000000),
 ( 0.9306880333625024981, 0.7472702456390875048, 1.000000000000000000),
 ( 0.9306880333625024981, 0.7472702456390875048, 1.000000000000000000) ) ) 
 REPRESENTATION_ITEM ( '' )  SURFACE ( )  );
#6649 = CARTESIAN_POINT ( 'NONE',  ( -40.43640613370507708, 9.999999999999998224, -157.5381262016859125 ) ) ;
#6650 = EDGE_CURVE ( 'NONE', #881, #13240, #12544, .T. ) ;
#6651 = CARTESIAN_POINT ( 'NONE',  ( 1.346194077712558279, 2.062500000000000000, -6.750000000000000888 ) ) ;
#6652 = VERTEX_POINT ( 'NONE', #6244 ) ;
#6653 = CARTESIAN_POINT ( 'NONE',  ( -10.59890792400177695, 9.999999999999998224, -125.3997871707501446 ) ) ;
#6654 = DIRECTION ( 'NONE',  ( 0.08794243244722427244, 0.000000000000000000, 0.9961255586397054218 ) ) ;
#6655 = CARTESIAN_POINT ( 'NONE',  ( 27.03835354040200301, 5.000000000000000888, -138.2189567750508843 ) ) ;
#6656 = CARTESIAN_POINT ( 'NONE',  ( -8.199037228205272143, 9.999999999999998224, -114.3845095685594515 ) ) ;
#6657 = CARTESIAN_POINT ( 'NONE',  ( -0.9685250182421367704, 1.734723475976807094E-15, -114.0968640496182758 ) ) ;
#6658 = CARTESIAN_POINT ( 'NONE',  ( -2.298097038856279362, 9.875000000000000000, -5.798097038856278473 ) ) ;
#6659 = CARTESIAN_POINT ( 'NONE',  ( 25.81993756852972055, 5.000000000000000888, -140.3392227823892711 ) ) ;
#6660 = CARTESIAN_POINT ( 'NONE',  ( 0.000000000000000000, 14.00000000000000000, 0.2500000000000002220 ) ) ;
#6661 = CARTESIAN_POINT ( 'NONE',  ( -63.31459619122251326, 14.99999999999999822, -201.9013287080907162 ) ) ;
#6662 = DIRECTION ( 'NONE',  ( -0.9510565162951478690, 0.000000000000000000, 0.3090169943749654369 ) ) ;
#6663 = CARTESIAN_POINT ( 'NONE',  ( 2.298097038856279362, 10.87500000000000178, -1.201902961143720860 ) ) ;
#6664 = CARTESIAN_POINT ( 'NONE',  ( -8.671560925439095513, 2.743867526398027223, -35.09585054340072219 ) ) ;
#6665 = CC_DESIGN_APPROVAL ( #10653, ( #8846 ) ) ;
#6666 = CARTESIAN_POINT ( 'NONE',  ( 4.912745175218361737, 14.82122587924934187, -0.1997555194214963581 ) ) ;
#6667 = CARTESIAN_POINT ( 'NONE',  ( -2.298097038856278473, 9.125000000000000000, -1.201902961143720416 ) ) ;
#6668 = CARTESIAN_POINT ( 'NONE',  ( 6.363274845737939778, 8.673617379884035472E-16, -132.2089327231069547 ) ) ;
#6669 = CARTESIAN_POINT ( 'NONE',  ( 26.58801926426209405, 5.000000000000000888, -139.0072983920785532 ) ) ;
#6670 = VERTEX_POINT ( 'NONE', #6078 ) ;
#6671 = EDGE_CURVE ( 'NONE', #2663, #4737, #2316, .T. ) ;
#6672 = CARTESIAN_POINT ( 'NONE',  ( 10.95703558056505500, 5.830465020145126687, -43.93897169094196187 ) ) ;
#6673 = CARTESIAN_POINT ( 'NONE',  ( 8.779290816849703916, 4.000000000000000888, -169.2528061090708036 ) ) ;
#6674 = CARTESIAN_POINT ( 'NONE',  ( 3.750000000000000000, 0.7500000000000000000, -3.500000000000000444 ) ) ;
#6675 = CARTESIAN_POINT ( 'NONE',  ( -4.592425496802573972E-16, 1.000000000000000000, -7.250000000000000000 ) ) ;
#6676 = ADVANCED_FACE ( 'NONE', ( #12028 ), #8818, .T. ) ;
#6677 = CARTESIAN_POINT ( 'NONE',  ( 3.249999999999998668, 1.687500000000000000, -4.846194077712560500 ) ) ;
#6678 = VERTEX_POINT ( 'NONE', #13524 ) ;
#6679 = CARTESIAN_POINT ( 'NONE',  ( 1.346194077712558057, 12.56250000000000000, -6.750000000000000000 ) ) ;
#6680 = DIRECTION ( 'NONE',  ( -1.000000000000000000, -0.000000000000000000, -0.000000000000000000 ) ) ;
#6681 = CARTESIAN_POINT ( 'NONE',  ( -0.3766621274091715987, 0.5000000000000000000, -7.146945437571387671 ) ) ;
#6682 = AXIS2_PLACEMENT_3D ( 'NONE', #8063, #12787, #4593 ) ;
#6683 = CIRCLE ( 'NONE', #7155, 3.500000000000000000 ) ;
#6684 = FACE_OUTER_BOUND ( 'NONE', #6011, .T. ) ;
#6685 = CARTESIAN_POINT ( 'NONE',  ( 6.122889832264990062, 5.000000000000000888, 5.281130614573720905 ) ) ;
#6686 = CARTESIAN_POINT ( 'NONE',  ( -9.678328886308937840, 10.72273131055397499, -116.3720502296813351 ) ) ;
#6687 = COORDINATED_UNIVERSAL_TIME_OFFSET ( 0, 0, .AHEAD. ) ;
#6688 = CARTESIAN_POINT ( 'NONE',  ( 11.86796838807922683, 14.99999999999814904, -123.5172601095007394 ) ) ;
#6689 = LINE ( 'NONE', #10311, #13589 ) ;
#6690 = CARTESIAN_POINT ( 'NONE',  ( 24.96080173480166664, 1.421781986531464703, -137.5233644729144089 ) ) ;
#6691 = ORIENTED_EDGE ( 'NONE', *, *, #2786, .F. ) ;
#6692 = AXIS2_PLACEMENT_3D ( 'NONE', #578, #2965, #8837 ) ;
#6693 = CARTESIAN_POINT ( 'NONE',  ( -3.249999999999999556, 3.312500000000000000, -4.846194077712557835 ) ) ;
#6694 = CARTESIAN_POINT ( 'NONE',  ( -30.70919553297256854, 4.000000000000000000, -193.1083921911521202 ) ) ;
#6695 = CARTESIAN_POINT ( 'NONE',  ( -3.749999999999999556, 3.750000000000000444, -3.499999999999999112 ) ) ;
#6696 = AXIS2_PLACEMENT_3D ( 'NONE', #2479, #11977, #1238 ) ;
#6697 = EDGE_CURVE ( 'NONE', #12980, #191, #6742, .T. ) ;
#6698 = VERTEX_POINT ( 'NONE', #5241 ) ;
#6699 = DIRECTION ( 'NONE',  ( 0.000000000000000000, 0.000000000000000000, 1.000000000000000000 ) ) ;
#6700 = CARTESIAN_POINT ( 'NONE',  ( -3.249999999999999556, 0.1875000000000000278, -2.153805922287440833 ) ) ;
#6701 = CARTESIAN_POINT ( 'NONE',  ( -2.651650429449552870, 6.125000000000000000, -0.8483495705504462414 ) ) ;
#6702 = VECTOR ( 'NONE', #9789, 1000.000000000000000 ) ;
#6703 = CARTESIAN_POINT ( 'NONE',  ( -25.11906781955737600, 1.301042606982605321E-15, -198.9681998140721078 ) ) ;
#6704 = CARTESIAN_POINT ( 'NONE',  ( -3.209935562023551459, -4.336808689942017736E-15, -120.5710852812284486 ) ) ;
#6705 = CARTESIAN_POINT ( 'NONE',  ( -2.651650429449553314, 3.375000000000000000, -6.151650429449552426 ) ) ;
#6706 = PERSON_AND_ORGANIZATION ( #3176, #3020 ) ;
#6707 = CARTESIAN_POINT ( 'NONE',  ( -4.975935430107378821, 0.000000000000000000, -1.000000000000001332 ) ) ;
#6708 = ORIENTED_EDGE ( 'NONE', *, *, #11316, .F. ) ;
#6709 = CARTESIAN_POINT ( 'NONE',  ( -1.346194077712559167, 3.937500000000000444, -6.749999999999999112 ) ) ;
#6710 =( GEOMETRIC_REPRESENTATION_CONTEXT ( 3 ) GLOBAL_UNCERTAINTY_ASSIGNED_CONTEXT ( ( #13624 ) ) GLOBAL_UNIT_ASSIGNED_CONTEXT ( ( #892, #13171, #2419 ) ) REPRESENTATION_CONTEXT ( 'NONE', 'WORKASPACE' ) );
#6711 = CARTESIAN_POINT ( 'NONE',  ( 9.926458935752712875, 14.67694112073403545, -106.4744043681741488 ) ) ;
#6712 = CARTESIAN_POINT ( 'NONE',  ( -2.651650429449552870, 10.62500000000000178, -0.8483495705504467965 ) ) ;
#6713 = CARTESIAN_POINT ( 'NONE',  ( 3.749999999999999556, 13.81250000000000000, -1.946699141100892261 ) ) ;
#6714 = CARTESIAN_POINT ( 'NONE',  ( -9.203922670347726154, 3.629878870852026651, -115.4376859600374416 ) ) ;
#6715 = ORIENTED_EDGE ( 'NONE', *, *, #10438, .T. ) ;
#6716 = DIRECTION ( 'NONE',  ( 0.8645818496218656835, 0.000000000000000000, -0.5024920151648518685 ) ) ;
#6717 = CARTESIAN_POINT ( 'NONE',  ( 2.298097038856278473, 8.625000000000000000, -5.798097038856279362 ) ) ;
#6718 = CARTESIAN_POINT ( 'NONE',  ( 3.749999999999999112, 10.18750000000000533, -5.053300858899108405 ) ) ;
#6719 = CARTESIAN_POINT ( 'NONE',  ( -3.849925124627588069, 4.336808689942017736E-16, -119.3240804248890612 ) ) ;
#6720 = CC_DESIGN_APPROVAL ( #10863, ( #1046 ) ) ;
#6721 = CARTESIAN_POINT ( 'NONE',  ( 4.529353718053118705, -2.743867526398026335, -43.69627513258503626 ) ) ;
#6722 = CARTESIAN_POINT ( 'NONE',  ( -0.2500000000000000555, 4.500000000000000888, -1.499999999999999778 ) ) ;
#6723 = ORIENTED_EDGE ( 'NONE', *, *, #6290, .T. ) ;
#6724 = CARTESIAN_POINT ( 'NONE',  ( -30.61853078688893248, 3.999999999999813483, -195.0175678202491554 ) ) ;
#6725 = DIRECTION ( 'NONE',  ( -0.9961255586397056438, 0.000000000000000000, 0.08794243244722428632 ) ) ;
#6726 = CARTESIAN_POINT ( 'NONE',  ( -33.77251566124539295, 15.00000000000000000, -156.1614337058108788 ) ) ;
#6727 = CARTESIAN_POINT ( 'NONE',  ( 1.346194077712561166, 2.437500000000000444, -0.2500000000000011102 ) ) ;
#6728 = ORIENTED_EDGE ( 'NONE', *, *, #9989, .T. ) ;
#6729 = CARTESIAN_POINT ( 'NONE',  ( -12.27209645382210113, 15.00000000000000000, -127.2227734861304782 ) ) ;
#6730 = LINE ( 'NONE', #6423, #7211 ) ;
#6731 = DIRECTION ( 'NONE',  ( -0.9999958530058989936, 0.000000000000000000, 0.002879925520664898108 ) ) ;
#6732 = CARTESIAN_POINT ( 'NONE',  ( 6.323089772814207699, 14.75164004108358640, 1.862046969705240640 ) ) ;
#6733 = CARTESIAN_POINT ( 'NONE',  ( -9.476787056091270145, 8.673617379884035472E-16, -115.4301398046334839 ) ) ;
#6734 = CARTESIAN_POINT ( 'NONE',  ( -3.980102097228897738E-16, 11.00000000000000178, -6.749999999999999112 ) ) ;
#6735 = CARTESIAN_POINT ( 'NONE',  ( -4.924771681124648026, 0.000000000000000000, -137.0932397189673111 ) ) ;
#6736 = CARTESIAN_POINT ( 'NONE',  ( 0.000000000000000000, 13.00000000000000178, 0.2500000000000002220 ) ) ;
#6737 = EDGE_CURVE ( 'NONE', #3762, #5120, #8310, .T. ) ;
#6738 = CIRCLE ( 'NONE', #6239, 2.000000000000000000 ) ;
#6739 = CYLINDRICAL_SURFACE ( 'NONE', #1739, 6.000000000000002665 ) ;
#6740 = CARTESIAN_POINT ( 'NONE',  ( -5.325284192974351960, 14.84655678240134868, -103.7367053080723593 ) ) ;
#6741 = CARTESIAN_POINT ( 'NONE',  ( -3.249999999999999556, 10.25000000000000000, -3.499999999999999556 ) ) ;
#6742 =( BOUNDED_CURVE ( )  B_SPLINE_CURVE ( 3, ( #3001, #12418, #610, #526 ),
 .UNSPECIFIED., .F., .F. ) 
 B_SPLINE_CURVE_WITH_KNOTS ( ( 4, 4 ),
 ( 2.332122453023544040, 2.380236920682249568 ),
 .UNSPECIFIED. ) 
 CURVE ( )  GEOMETRIC_REPRESENTATION_ITEM ( )  RATIONAL_B_SPLINE_CURVE ( ( 1.000000000000000000, 0.9998070924708732932, 0.9998070924708732932, 1.000000000000000000 ) ) 
 REPRESENTATION_ITEM ( '' )  );
#6743 = CARTESIAN_POINT ( 'NONE',  ( -5.388443496774984354, 10.00000000000000178, -115.7979535283634931 ) ) ;
#6744 = DIRECTION ( 'NONE',  ( 0.000000000000000000, 0.000000000000000000, -1.000000000000000000 ) ) ;
#6745 = CARTESIAN_POINT ( 'NONE',  ( 1.346194077712560944, 7.937500000000000888, -0.2500000000000010547 ) ) ;
#6746 = CARTESIAN_POINT ( 'NONE',  ( 3.226485357636315499, 4.342686168579469097, 5.175911514346425157 ) ) ;
#6747 = CARTESIAN_POINT ( 'NONE',  ( 9.939878312292615092, 5.000000000000000888, -115.2320631035898373 ) ) ;
#6748 = EDGE_LOOP ( 'NONE', ( #8201, #4016, #14040, #8767 ) ) ;
#6749 = EDGE_LOOP ( 'NONE', ( #14946, #3203 ) ) ;
#6750 = CARTESIAN_POINT ( 'NONE',  ( 4.624333745513747651, 15.00000000000000000, -103.8844720882033954 ) ) ;
#6751 = CARTESIAN_POINT ( 'NONE',  ( 3.749999999999998668, 2.687500000000000888, -5.053300858899107517 ) ) ;
#6752 = VECTOR ( 'NONE', #5070, 1000.000000000000000 ) ;
#6753 = CARTESIAN_POINT ( 'NONE',  ( -3.249999999999999556, 13.75000000000000000, -3.500000000000000000 ) ) ;
#6754 = CARTESIAN_POINT ( 'NONE',  ( 12.93066528927006331, 3.999999999993260502, -166.5029444825368614 ) ) ;
#6755 = ORIENTED_EDGE ( 'NONE', *, *, #14418, .T. ) ;
#6756 = CARTESIAN_POINT ( 'NONE',  ( 1.346194077712558057, 10.56250000000000000, -6.750000000000000000 ) ) ;
#6757 = CARTESIAN_POINT ( 'NONE',  ( -3.213772066606566558, -2.558678233169556115, -1.000000000000011990 ) ) ;
#6758 = CARTESIAN_POINT ( 'NONE',  ( -7.646413850410871405, 13.39228090183835285, -104.8572026217608482 ) ) ;
#6759 = EDGE_CURVE ( 'NONE', #10593, #1043, #9903, .T. ) ;
#6760 =( NAMED_UNIT ( * ) SI_UNIT ( $, .STERADIAN. ) SOLID_ANGLE_UNIT ( ) );
#6761 = AXIS2_PLACEMENT_3D ( 'NONE', #12194, #9803, #6158 ) ;
#6762 = APPROVAL_ROLE ( '' ) ;
#6763 = VECTOR ( 'NONE', #9339, 1000.000000000000000 ) ;
#6764 = CARTESIAN_POINT ( 'NONE',  ( 7.523470539541117219, 15.00000000000000000, -107.6366068479289311 ) ) ;
#6765 = FACE_OUTER_BOUND ( 'NONE', #1736, .T. ) ;
#6766 = ORIENTED_EDGE ( 'NONE', *, *, #12216, .F. ) ;
#6767 = CARTESIAN_POINT ( 'NONE',  ( 25.97223239244240389, 2.194422113489858717, -138.3554727711511134 ) ) ;
#6768 = CARTESIAN_POINT ( 'NONE',  ( -3.249999999999999556, 9.250000000000000000, -3.499999999999999556 ) ) ;
#6769 = VERTEX_POINT ( 'NONE', #1069 ) ;
#6770 = CARTESIAN_POINT ( 'NONE',  ( -2.298097038856278918, 4.375000000000000000, -5.798097038856277585 ) ) ;
#6771 = CARTESIAN_POINT ( 'NONE',  ( -16.34918561525985936, 4.000000000000000888, -155.5261654759235057 ) ) ;
#6772 = CARTESIAN_POINT ( 'NONE',  ( 3.749999999999999112, 0.1875000000000000833, -5.053300858899108405 ) ) ;
#6773 = EDGE_LOOP ( 'NONE', ( #12346, #9013, #4589, #2604 ) ) ;
#6774 = FACE_OUTER_BOUND ( 'NONE', #11730, .T. ) ;
#6775 = AXIS2_PLACEMENT_3D ( 'NONE', #12947, #9376, #3590 ) ;
#6776 = CARTESIAN_POINT ( 'NONE',  ( 3.249999999999999556, 0.7500000000000000000, -3.500000000000000000 ) ) ;
#6777 = CARTESIAN_POINT ( 'NONE',  ( -3.749999999999999556, 5.312500000000001776, -5.053300858899104853 ) ) ;
#6778 = CARTESIAN_POINT ( 'NONE',  ( -25.11906781955737600, 1.301042606982605321E-15, -198.9681998140721078 ) ) ;
#6779 = EDGE_CURVE ( 'NONE', #3495, #13258, #4048, .T. ) ;
#6780 = CARTESIAN_POINT ( 'NONE',  ( -1.947391641747792779, -6.071532165918824830E-15, -123.5657085572418339 ) ) ;
#6781 = EDGE_CURVE ( 'NONE', #2896, #8666, #8471, .T. ) ;
#6782 = APPROVAL_ROLE ( '' ) ;
#6783 = ADVANCED_FACE ( 'NONE', ( #903 ), #12657, .F. ) ;
#6784 = CARTESIAN_POINT ( 'NONE',  ( 1.266169042200451900, 4.000000000000000000, -139.9015330219193913 ) ) ;
#6785 = CIRCLE ( 'NONE', #14704, 11.99999999999995559 ) ;
#6786 = ORIENTED_EDGE ( 'NONE', *, *, #837, .F. ) ;
#6787 = APPROVAL ( #13274, 'UNSPECIFIED' ) ;
#6788 = CARTESIAN_POINT ( 'NONE',  ( 3.249999999999999556, 9.250000000000001776, -3.500000000000000000 ) ) ;
#6789 = DIRECTION ( 'NONE',  ( 0.000000000000000000, 1.000000000000000000, 0.000000000000000000 ) ) ;
#6790 = CARTESIAN_POINT ( 'NONE',  ( 1.553300858899109071, 10.43750000000000178, 0.2499999999999989175 ) ) ;
#6791 = CARTESIAN_POINT ( 'NONE',  ( 0.000000000000000000, 15.00000000000000000, 0.2500000000000002220 ) ) ;
#6792 = ORIENTED_EDGE ( 'NONE', *, *, #2974, .T. ) ;
#6793 = CARTESIAN_POINT ( 'NONE',  ( -1.813969075506799422, 7.379999999999995453, -48.97454890480479861 ) ) ;
#6794 = CARTESIAN_POINT ( 'NONE',  ( 2.298097038856278473, 7.625000000000000000, -5.798097038856279362 ) ) ;
#6795 = CARTESIAN_POINT ( 'NONE',  ( -3.249999999999999112, -0.3124999999999999445, -2.153805922287440833 ) ) ;
#6796 = CARTESIAN_POINT ( 'NONE',  ( 10.90625579228518838, 8.773889247172311556, -41.61220587883767053 ) ) ;
#6797 = DIRECTION ( 'NONE',  ( -0.5109044416013800438, -0.8090169943749470072, 0.2906340557548426906 ) ) ;
#6798 = EDGE_LOOP ( 'NONE', ( #1641, #7056, #13182, #301 ) ) ;
#6799 = CARTESIAN_POINT ( 'NONE',  ( -26.63481489508266975, 3.005459392714369724E-12, -206.0878104404494309 ) ) ;
#6800 = CARTESIAN_POINT ( 'NONE',  ( -59.92301775443486633, 15.00000000000000000, -171.2216082921338227 ) ) ;
#6801 = CARTESIAN_POINT ( 'NONE',  ( -3.249999999999999112, 1.687500000000000222, -2.153805922287440833 ) ) ;
#6802 = ORIENTED_EDGE ( 'NONE', *, *, #12814, .T. ) ;
#6803 = CARTESIAN_POINT ( 'NONE',  ( -10.59890792386395475, 14.99999999999880629, -125.3997871708591703 ) ) ;
#6804 = CARTESIAN_POINT ( 'NONE',  ( 6.089666224640344794, 15.00000000000000000, -124.6062682140657074 ) ) ;
#6805 = CARTESIAN_POINT ( 'NONE',  ( 8.983555716587311224, 12.48436874840615474, 0.6556481286397073394 ) ) ;
#6806 = CARTESIAN_POINT ( 'NONE',  ( -3.294555838623477229, 1.734723475976807094E-15, -108.9576586821670929 ) ) ;
#6807 = CARTESIAN_POINT ( 'NONE',  ( -2.298097038856278029, 13.62500000000000000, -1.201902961143720638 ) ) ;
#6808 = DIRECTION ( 'NONE',  ( -0.08794243244722427244, 0.000000000000000000, -0.9961255586397055328 ) ) ;
#6809 = CARTESIAN_POINT ( 'NONE',  ( 2.651650429449552870, 2.125000000000000000, -6.151650429449555091 ) ) ;
#6810 = DIRECTION ( 'NONE',  ( 0.08794243244722427244, 0.000000000000000000, 0.9961255586397055328 ) ) ;
#6811 = LINE ( 'NONE', #9207, #12848 ) ;
#6812 = FACE_OUTER_BOUND ( 'NONE', #1871, .T. ) ;
#6813 = CARTESIAN_POINT ( 'NONE',  ( 1.320501113854927633, 6.000000000000000000, -137.8664870916819893 ) ) ;
#6814 = CARTESIAN_POINT ( 'NONE',  ( -3.249999999999999556, 9.312499999999998224, -4.846194077712557835 ) ) ;
#6815 = CARTESIAN_POINT ( 'NONE',  ( 3.212062097439680741, 3.696815382486504653, 5.047156548192035963 ) ) ;
#6816 = CARTESIAN_POINT ( 'NONE',  ( -9.721966606378851239, 10.00000000000000000, -116.3614657639809309 ) ) ;
#6817 = EDGE_LOOP ( 'NONE', ( #2512, #9442, #10931, #10854 ) ) ;
#6818 = B_SPLINE_SURFACE_WITH_KNOTS ( 'NONE', 1, 3, ( 
 ( #8889, #11133, #4034, #1784, #8739, #12445, #4183, #11212, #8963, #1865 ),
 ( #5409, #7805, #551, #5264, #8657, #13470, #6493, #12218, #2873, #6644 ) ),
 .UNSPECIFIED., .F., .F., .F.,
 ( 2, 2 ),
 ( 4, 2, 2, 2, 4 ),
 ( 0.000000000000000000, 1.000000000000000000 ),
 ( 1.315450245614885549, 1.577474171769009281, 1.839498097923133013, 2.101522024077256745, 2.363545950231380477 ),
 .UNSPECIFIED. ) ;
#6819 = VERTEX_POINT ( 'NONE', #13663 ) ;
#6820 = CARTESIAN_POINT ( 'NONE',  ( 2.112978062913205779, 8.673617379884035472E-16, -168.2508114127782903 ) ) ;
#6821 = CARTESIAN_POINT ( 'NONE',  ( 3.749999999999999112, 0.8125000000000001110, -1.946699141100892039 ) ) ;
#6822 = CARTESIAN_POINT ( 'NONE',  ( -1.346194077712559167, 13.93750000000000000, -6.749999999999999112 ) ) ;
#6823 = CARTESIAN_POINT ( 'NONE',  ( -8.602511405380996123, 2.500000000000000444, -105.7492080835845485 ) ) ;
#6824 = EDGE_LOOP ( 'NONE', ( #3989, #268, #2356 ) ) ;
#6825 = CARTESIAN_POINT ( 'NONE',  ( -1.346194077712558945, 1.562500000000000222, -0.2500000000000002220 ) ) ;
#6826 = CARTESIAN_POINT ( 'NONE',  ( 30.99422529207408772, 8.773889247172311556, -45.42481409048903629 ) ) ;
#6827 = CARTESIAN_POINT ( 'NONE',  ( -8.357321192833575552, 12.30945435311018521, -105.2297795656583759 ) ) ;
#6828 = CARTESIAN_POINT ( 'NONE',  ( -3.249999999999999556, 3.312500000000000000, -4.846194077712557835 ) ) ;
#6829 = ITEM_DEFINED_TRANSFORMATION ( 'NONE', 'NONE', #11879,  #9419 ) ;
#6830 = CARTESIAN_POINT ( 'NONE',  ( 8.428994341650765776, 12.49999999999999822, -112.3028785388504218 ) ) ;
#6831 = CARTESIAN_POINT ( 'NONE',  ( -6.572203743845812518, 14.53696891565361327, -117.0568686706825332 ) ) ;
#6832 = ORIENTED_EDGE ( 'NONE', *, *, #164, .F. ) ;
#6833 = CARTESIAN_POINT ( 'NONE',  ( 26.90873434660125341, 2.875118758487606563, -137.5417689853771606 ) ) ;
#6834 = CARTESIAN_POINT ( 'NONE',  ( 1.346194077712560944, 10.93750000000000178, -0.2500000000000011102 ) ) ;
#6835 = VERTEX_POINT ( 'NONE', #3064 ) ;
#6836 = ORIENTED_EDGE ( 'NONE', *, *, #7622, .T. ) ;
#6837 = CARTESIAN_POINT ( 'NONE',  ( 1.553300858899109516, 11.43750000000000178, 0.2499999999999993616 ) ) ;
#6838 = DIRECTION ( 'NONE',  ( 0.9997619372588930631, 0.000000000000000000, 0.02181900108494949642 ) ) ;
#6839 = CARTESIAN_POINT ( 'NONE',  ( -1.553300858899106629, 0.5625000000000003331, 0.2500000000000002220 ) ) ;
#6840 = CIRCLE ( 'NONE', #3627, 0.2500000000000002220 ) ;
#6841 = CARTESIAN_POINT ( 'NONE',  ( 3.249999999999999556, 5.250000000000000000, -3.500000000000000000 ) ) ;
#6842 = ORIENTED_EDGE ( 'NONE', *, *, #11652, .F. ) ;
#6843 = EDGE_CURVE ( 'NONE', #7860, #11175, #4306, .T. ) ;
#6844 = DIRECTION ( 'NONE',  ( 0.000000000000000000, 1.000000000000000000, 0.000000000000000000 ) ) ;
#6845 = CARTESIAN_POINT ( 'NONE',  ( -1.346194077712559389, 3.062500000000000000, -0.2500000000000002220 ) ) ;
#6846 = CARTESIAN_POINT ( 'NONE',  ( -1.553300858899106629, 7.062500000000000000, 0.2500000000000002220 ) ) ;
#6847 = B_SPLINE_CURVE_WITH_KNOTS ( 'NONE', 3,
 ( #6978, #8210, #2417, #12709, #10536, #11762, #12941, #11542, #10464, #1182, #15269, #15122, #14180, #5965, #14254, #2122, #3585, #957 ),
 .UNSPECIFIED., .F., .F.,
 ( 4, 2, 2, 2, 2, 2, 2, 2, 4 ),
 ( 1.734723475976807094E-18, 0.004481983308881167319, 0.006722974963321751846, 0.008963966617762334638, 0.01120495827220291916, 0.01344594992664350716, 0.01456644575386379682, 0.01568694158108408648, 0.01792793323552462764 ),
 .UNSPECIFIED. ) ;
#6848 = CARTESIAN_POINT ( 'NONE',  ( -25.44770677137621107, 3.658198091069090996, -208.9169813633941430 ) ) ;
#6849 = LINE ( 'NONE', #3523, #8929 ) ;
#6850 = CC_DESIGN_PERSON_AND_ORGANIZATION_ASSIGNMENT ( #14532, #8629, ( #2984 ) ) ;
#6851 = CALENDAR_DATE ( 2026, 8, 10 ) ;
#6852 = CARTESIAN_POINT ( 'NONE',  ( 10.42535907228127279, 5.000000000000000000, -121.1971725648922700 ) ) ;
#6853 = CARTESIAN_POINT ( 'NONE',  ( 30.96695154071790412, 8.773889247172311556, -44.17511166891541308 ) ) ;
#6854 = EDGE_LOOP ( 'NONE', ( #11660, #3670, #14559, #10602 ) ) ;
#6855 = CARTESIAN_POINT ( 'NONE',  ( -3.249999999999999556, 8.750000000000001776, -3.500000000000000000 ) ) ;
#6856 = EDGE_CURVE ( 'NONE', #11095, #5602, #8737, .T. ) ;
#6857 = DIRECTION ( 'NONE',  ( 1.000000000000000000, 0.000000000000000000, -8.764770998266003672E-18 ) ) ;
#6858 = ADVANCED_FACE ( 'NONE', ( #5604 ), #7775, .F. ) ;
#6859 = CARTESIAN_POINT ( 'NONE',  ( -1.553300858899106629, 9.562500000000000000, 0.2499999999999998335 ) ) ;
#6860 = CARTESIAN_POINT ( 'NONE',  ( -1.553300858899107073, 13.43750000000000000, -7.250000000000000000 ) ) ;
#6861 = CARTESIAN_POINT ( 'NONE',  ( -65.78451708959967448, 14.92583229181892612, -188.0906790823463268 ) ) ;
#6862 = CARTESIAN_POINT ( 'NONE',  ( 0.7644969749118040170, 5.000000000000000000, -138.4027240657576101 ) ) ;
#6863 = CARTESIAN_POINT ( 'NONE',  ( 2.651650429449552870, 13.12499999999999822, -6.151650429449555091 ) ) ;
#6864 = CARTESIAN_POINT ( 'NONE',  ( -10.02475322368603194, 5.000000000000000000, -286.9457450322071281 ) ) ;
#6865 = DATE_AND_TIME ( #2313, #6956 ) ;
#6866 = DIRECTION ( 'NONE',  ( 0.9207838613340401102, 0.000000000000000000, -0.3900731735287307211 ) ) ;
#6867 = ORIENTED_EDGE ( 'NONE', *, *, #14255, .T. ) ;
#6868 = CARTESIAN_POINT ( 'NONE',  ( -28.93490687045225229, 4.000000000000780709, -203.2856232654508517 ) ) ;
#6869 = CARTESIAN_POINT ( 'NONE',  ( -3.249999999999999556, 4.187500000000000000, -2.153805922287440833 ) ) ;
#6870 = CARTESIAN_POINT ( 'NONE',  ( -60.74056104668384393, 9.999999999999998224, -188.2485173983553466 ) ) ;
#6871 = CARTESIAN_POINT ( 'NONE',  ( -3.980102097228897738E-16, 2.000000000000000000, -6.749999999999999112 ) ) ;
#6872 = ORIENTED_EDGE ( 'NONE', *, *, #13598, .F. ) ;
#6873 = CARTESIAN_POINT ( 'NONE',  ( 3.136841903360911843, 5.000000000000000888, -104.4936450199714812 ) ) ;
#6874 = EDGE_CURVE ( 'NONE', #14600, #5913, #5525, .T. ) ;
#6875 = CARTESIAN_POINT ( 'NONE',  ( -25.45473766001728322, 3.555369740890242269, -208.8630699688340826 ) ) ;
#6876 = CARTESIAN_POINT ( 'NONE',  ( 8.899585189996612300, 13.22278168266239717, 4.503236568198851764 ) ) ;
#6877 = CARTESIAN_POINT ( 'NONE',  ( -0.8896971555406301135, 5.000000000000000888, -104.6801027822243100 ) ) ;
#6878 = CARTESIAN_POINT ( 'NONE',  ( -1.346194077712559167, 10.93750000000000355, -6.749999999999999112 ) ) ;
#6879 = CARTESIAN_POINT ( 'NONE',  ( 15.16156648847430688, 6.947217876059453517E-12, -161.5519024490983213 ) ) ;
#6880 = CARTESIAN_POINT ( 'NONE',  ( -2.651650429449553314, 2.875000000000000000, -6.151650429449552426 ) ) ;
#6881 = DIRECTION ( 'NONE',  ( -0.05964429961207245307, 0.000000000000000000, -0.9982196940171964572 ) ) ;
#6882 = DIRECTION ( 'NONE',  ( 0.9876883405951377704, 0.000000000000000000, 0.1564344650402315628 ) ) ;
#6883 = CARTESIAN_POINT ( 'NONE',  ( 26.71007981443199952, 5.000000000000000888, -136.8791680534710054 ) ) ;
#6884 = CYLINDRICAL_SURFACE ( 'NONE', #6028, 3.500000000000013323 ) ;
#6885 = CARTESIAN_POINT ( 'NONE',  ( 3.249999999999999112, 9.812500000000000000, -2.153805922287439945 ) ) ;
#6886 = DIRECTION ( 'NONE',  ( 0.000000000000000000, -1.000000000000000000, 0.000000000000000000 ) ) ;
#6887 = LINE ( 'NONE', #1026, #14077 ) ;
#6888 = ORIENTED_EDGE ( 'NONE', *, *, #7120, .F. ) ;
#6889 = ORIENTED_EDGE ( 'NONE', *, *, #224, .F. ) ;
#6890 = CARTESIAN_POINT ( 'NONE',  ( 5.147364755317443752, 4.000000000000000000, -172.0982971393951289 ) ) ;
#6891 = CARTESIAN_POINT ( 'NONE',  ( 1.553300858899105963, 6.562500000000000000, -7.250000000000000888 ) ) ;
#6892 = CARTESIAN_POINT ( 'NONE',  ( 1.346194077712558279, 15.06250000000000178, -6.750000000000000888 ) ) ;
#6893 = CARTESIAN_POINT ( 'NONE',  ( -6.488009013026156957, 4.336808689942017736E-16, -104.2969138198227910 ) ) ;
#6894 = ORIENTED_EDGE ( 'NONE', *, *, #8374, .T. ) ;
#6895 = CARTESIAN_POINT ( 'NONE',  ( 3.249999999999998668, 14.68750000000000000, -4.846194077712560500 ) ) ;
#6896 = CARTESIAN_POINT ( 'NONE',  ( -47.48189921986828921, 15.00000000000000000, -141.5723758807981483 ) ) ;
#6897 = APPROVAL_PERSON_ORGANIZATION ( #3840, #6787, #442 ) ;
#6898 = CARTESIAN_POINT ( 'NONE',  ( -8.659743771704308202, 12.30945435306794877, -104.4813518601836790 ) ) ;
#6899 =( NAMED_UNIT ( * ) SI_UNIT ( $, .STERADIAN. ) SOLID_ANGLE_UNIT ( ) );
#6900 = CARTESIAN_POINT ( 'NONE',  ( 2.298097038856278473, 3.625000000000000000, -5.798097038856279362 ) ) ;
#6901 = CIRCLE ( 'NONE', #11352, 0.4999999999999726885 ) ;
#6902 = PERSON_AND_ORGANIZATION ( #13323, #5681 ) ;
#6903 = CARTESIAN_POINT ( 'NONE',  ( 10.14688567197878477, 15.00000000000115996, -108.1982192591100755 ) ) ;
#6904 = CYLINDRICAL_SURFACE ( 'NONE', #4206, 3.000000000000002665 ) ;
#6905 = ORIENTED_EDGE ( 'NONE', *, *, #11967, .T. ) ;
#6906 = DIRECTION ( 'NONE',  ( -0.000000000000000000, 1.000000000000000000, -0.000000000000000000 ) ) ;
#6907 = CARTESIAN_POINT ( 'NONE',  ( 3.249999999999999112, 12.81250000000000178, -2.153805922287439945 ) ) ;
#6908 = VERTEX_POINT ( 'NONE', #4451 ) ;
#6909 = ORIENTED_EDGE ( 'NONE', *, *, #3291, .T. ) ;
#6910 = CARTESIAN_POINT ( 'NONE',  ( 2.651650429449552870, 8.125000000000000000, -6.151650429449555091 ) ) ;
#6911 = CARTESIAN_POINT ( 'NONE',  ( -3.125658737029940681, 2.331468351712828833E-16, 3.587914672538146554 ) ) ;
#6912 = CARTESIAN_POINT ( 'NONE',  ( -1.553300858899106629, 6.562500000000000888, 0.2500000000000002220 ) ) ;
#6913 = CARTESIAN_POINT ( 'NONE',  ( -1.346194077712559167, 4.937500000000000888, -6.749999999999999112 ) ) ;
#6914 = VERTEX_POINT ( 'NONE', #2135 ) ;
#6915 = ORGANIZATION ( 'NAUO-ORG6', 'UNSPECIFIED', 'UNSPECIFIED' ) ;
#6916 = CARTESIAN_POINT ( 'NONE',  ( -1.030030361948892192, 9.999999999999998224, -105.0143096064267780 ) ) ;
#6917 = CARTESIAN_POINT ( 'NONE',  ( -2.298097038856278918, 1.375000000000000000, -5.798097038856277585 ) ) ;
#6918 = AXIS2_PLACEMENT_3D ( 'NONE', #11916, #6045, #14652 ) ;
#6919 = CARTESIAN_POINT ( 'NONE',  ( 1.553300858899105963, 4.562500000000000888, -7.250000000000000888 ) ) ;
#6920 = CARTESIAN_POINT ( 'NONE',  ( -25.07851259296351643, 1.351337947789349903, -206.3038523730356815 ) ) ;
#6921 = DIRECTION ( 'NONE',  ( 0.02181900108494707127, 0.000000000000000000, -0.9997619372588931741 ) ) ;
#6922 = ADVANCED_FACE ( 'NONE', ( #6620 ), #3135, .T. ) ;
#6923 = CALENDAR_DATE ( 2026, 8, 10 ) ;
#6924 = AXIS2_PLACEMENT_3D ( 'NONE', #12, #10674, #1100 ) ;
#6925 = EDGE_CURVE ( 'NONE', #673, #40, #13089, .T. ) ;
#6926 = LINE ( 'NONE', #1204, #6287 ) ;
#6927 = VECTOR ( 'NONE', #10209, 1000.000000000000000 ) ;
#6928 = CARTESIAN_POINT ( 'NONE',  ( 30.96695154071790412, 8.773889247172311556, -44.17511166891541308 ) ) ;
#6929 = VERTEX_POINT ( 'NONE', #9467 ) ;
#6930 = CARTESIAN_POINT ( 'NONE',  ( 3.249999999999998224, 8.187500000000000000, -4.846194077712561388 ) ) ;
#6931 = LINE ( 'NONE', #8017, #12170 ) ;
#6932 = AXIS2_PLACEMENT_3D ( 'NONE', #7818, #2954, #9126 ) ;
#6933 = CARTESIAN_POINT ( 'NONE',  ( -1.553300858899107073, 9.937500000000001776, -7.249999999999999112 ) ) ;
#6934 = CARTESIAN_POINT ( 'NONE',  ( 1.553300858899108849, 13.93750000000000000, 0.2499999999999993616 ) ) ;
#6935 = CARTESIAN_POINT ( 'NONE',  ( -64.60583417973334974, 13.85924130109725283, -199.3306212659461494 ) ) ;
#6936 = CARTESIAN_POINT ( 'NONE',  ( -0.8169061489538727017, 1.565995602528241992, -138.1029328351367553 ) ) ;
#6937 = CARTESIAN_POINT ( 'NONE',  ( -4.592425496802573972E-16, 13.00000000000000000, -7.250000000000000000 ) ) ;
#6938 = FACE_OUTER_BOUND ( 'NONE', #1919, .T. ) ;
#6939 = PERSON_AND_ORGANIZATION ( #3176, #3020 ) ;
#6940 = EDGE_CURVE ( 'NONE', #10699, #1764, #3667, .T. ) ;
#6941 = EDGE_CURVE ( 'NONE', #14015, #6908, #1827, .T. ) ;
#6942 = CARTESIAN_POINT ( 'NONE',  ( 5.228075279701640099, 1.000000000000000000, -167.7939279834373849 ) ) ;
#6943 = AXIS2_PLACEMENT_3D ( 'NONE', #11949, #8549, #13125 ) ;
#6944 = ORIENTED_EDGE ( 'NONE', *, *, #5263, .T. ) ;
#6945 = CARTESIAN_POINT ( 'NONE',  ( -23.88626836071575354, 8.673617379884035472E-16, -202.5895577731797061 ) ) ;
#6946 = CARTESIAN_POINT ( 'NONE',  ( 1.346194077712558279, 4.562500000000001776, -6.750000000000000000 ) ) ;
#6947 = CARTESIAN_POINT ( 'NONE',  ( -68.00022065852073183, 15.00000000000000000, -200.6045152126381197 ) ) ;
#6948 = CARTESIAN_POINT ( 'NONE',  ( -3.249999999999999556, 3.750000000000000444, -3.500000000000000000 ) ) ;
#6949 = ORIENTED_EDGE ( 'NONE', *, *, #9600, .T. ) ;
#6950 = DIRECTION ( 'NONE',  ( 1.000000000000000000, 0.000000000000000000, 0.000000000000000000 ) ) ;
#6951 = DIRECTION ( 'NONE',  ( -0.9997619372588932851, -0.000000000000000000, -0.02181900108494707821 ) ) ;
#6952 = CARTESIAN_POINT ( 'NONE',  ( 8.921562004896541609, 14.16567896455317843, 3.496243491202363440 ) ) ;
#6953 = CARTESIAN_POINT ( 'NONE',  ( -1.334601435094046273, 8.673617379884035472E-16, -105.6792246796767074 ) ) ;
#6954 = CARTESIAN_POINT ( 'NONE',  ( 3.249999999999998224, 11.31250000000000355, -2.153805922287439945 ) ) ;
#6955 = CC_DESIGN_PERSON_AND_ORGANIZATION_ASSIGNMENT ( #12404, #6614, ( #10116 ) ) ;
#6956 = LOCAL_TIME ( 12, 28, 20.00000000000000000, #14286 ) ;
#6957 = LINE ( 'NONE', #4643, #12631 ) ;
#6958 = CARTESIAN_POINT ( 'NONE',  ( 3.749999999999999556, 2.249999999999999556, -3.500000000000000444 ) ) ;
#6959 = DIRECTION ( 'NONE',  ( -0.000000000000000000, -1.000000000000000000, -0.000000000000000000 ) ) ;
#6960 = CARTESIAN_POINT ( 'NONE',  ( 27.03835354040190708, 6.000000000000000000, -138.2189567750509696 ) ) ;
#6961 = ADVANCED_FACE ( 'NONE', ( #8074 ), #1353, .T. ) ;
#6962 = ADVANCED_FACE ( 'NONE', ( #8369 ), #5977, .T. ) ;
#6963 = CARTESIAN_POINT ( 'NONE',  ( 26.07883353259989434, 2.736193318683750597, -137.1131491302461995 ) ) ;
#6964 = EDGE_CURVE ( 'NONE', #11483, #14924, #2560, .T. ) ;
#6965 = CARTESIAN_POINT ( 'NONE',  ( -1.160594694320683518, 0.000000000000000000, 0.5210215923759190515 ) ) ;
#6966 = CARTESIAN_POINT ( 'NONE',  ( -3.980102097228897245E-16, 14.50000000000000000, -6.749999999999999112 ) ) ;
#6967 = CARTESIAN_POINT ( 'NONE',  ( 3.221353676048400061, 14.96825566296426935, -12.98096750502963381 ) ) ;
#6968 = CARTESIAN_POINT ( 'NONE',  ( -63.60348060676458459, 15.00000000000000000, -180.2685449772604045 ) ) ;
#6969 = ORIENTED_EDGE ( 'NONE', *, *, #8776, .F. ) ;
#6970 = ORIENTED_EDGE ( 'NONE', *, *, #625, .F. ) ;
#6971 = CARTESIAN_POINT ( 'NONE',  ( -10.64937093114562217, 4.000000000002276401, -187.1793336183638985 ) ) ;
#6972 = CARTESIAN_POINT ( 'NONE',  ( -4.592425496802573972E-16, 4.500000000000000888, -7.249999999999999112 ) ) ;
#6973 = CARTESIAN_POINT ( 'NONE',  ( -2.651650429449552870, 4.624999999999999112, -0.8483495705504467965 ) ) ;
#6974 = CARTESIAN_POINT ( 'NONE',  ( 4.047901359262597865, 14.99999999996766675, -106.4041221357216216 ) ) ;
#6975 = ORIENTED_EDGE ( 'NONE', *, *, #12555, .F. ) ;
#6976 = CIRCLE ( 'NONE', #8483, 2.000000000000001776 ) ;
#6977 = CARTESIAN_POINT ( 'NONE',  ( 3.249999999999999112, 13.81250000000000000, -2.153805922287439945 ) ) ;
#6978 = CARTESIAN_POINT ( 'NONE',  ( -9.385448347264267355, 5.000000000000000888, -115.3551636530117150 ) ) ;
#6979 = B_SPLINE_CURVE_WITH_KNOTS ( 'NONE', 3,
 ( #4963, #7110, #410, #249, #9678, #14409, #14324, #1412, #3649, #2650 ),
 .UNSPECIFIED., .F., .F.,
 ( 4, 2, 2, 2, 4 ),
 ( 0.002313672523134014964, 0.002886887860852135976, 0.003460103198570256555, 0.004033318536288377568, 0.004606533874006498580 ),
 .UNSPECIFIED. ) ;
#6980 = CARTESIAN_POINT ( 'NONE',  ( -8.201734205038356151, 12.60136528525868371, -105.1471006946589881 ) ) ;
#6981 = CARTESIAN_POINT ( 'NONE',  ( -2.298097038856278473, 2.125000000000000000, -1.201902961143720416 ) ) ;
#6982 = PERSON_AND_ORGANIZATION ( #4286, #13353 ) ;
#6983 = CARTESIAN_POINT ( 'NONE',  ( 11.13433036043491242, 15.00000000000000000, -107.0267359326556971 ) ) ;
#6984 = CARTESIAN_POINT ( 'NONE',  ( 16.81337476694494626, 0.000000000000000000, -129.2521154344591139 ) ) ;
#6985 = VERTEX_POINT ( 'NONE', #1125 ) ;
#6986 = CIRCLE ( 'NONE', #8463, 2.000000000000000000 ) ;
#6987 = CARTESIAN_POINT ( 'NONE',  ( -0.8709518826452680162, 14.99999999999999645, -118.3049497858321217 ) ) ;
#6988 = CARTESIAN_POINT ( 'NONE',  ( -2.298097038856278473, 10.12500000000000000, -1.201902961143720416 ) ) ;
#6989 = ORIENTED_EDGE ( 'NONE', *, *, #8941, .F. ) ;
#6990 = ORIENTED_EDGE ( 'NONE', *, *, #647, .F. ) ;
#6991 = CARTESIAN_POINT ( 'NONE',  ( -25.42939282183900573, 4.000000000000000000, -209.0516719515502473 ) ) ;
#6992 = CARTESIAN_POINT ( 'NONE',  ( -2.651650429449553314, 4.875000000000000000, -6.151650429449552426 ) ) ;
#6993 = CARTESIAN_POINT ( 'NONE',  ( 3.249999999999998224, 7.187500000000000888, -4.846194077712561388 ) ) ;
#6994 = ORIENTED_EDGE ( 'NONE', *, *, #15170, .T. ) ;
#6995 = CARTESIAN_POINT ( 'NONE',  ( -3.294555838741347831, 9.999999999999998224, -108.9576586820926281 ) ) ;
#6996 = CARTESIAN_POINT ( 'NONE',  ( -2.298097038856278473, 2.125000000000000000, -1.201902961143720416 ) ) ;
#6997 = CARTESIAN_POINT ( 'NONE',  ( 3.749999999999999112, 9.812500000000000000, -1.946699141100892039 ) ) ;
#6998 = AXIS2_PLACEMENT_3D ( 'NONE', #14491, #14247, #8352 ) ;
#6999 = CARTESIAN_POINT ( 'NONE',  ( -25.58997729346963013, 2.130041082828657562, -207.6174152824262080 ) ) ;
#7000 = FACE_OUTER_BOUND ( 'NONE', #13338, .T. ) ;
#7001 = DIRECTION ( 'NONE',  ( -0.000000000000000000, -1.000000000000000000, -0.000000000000000000 ) ) ;
#7002 = APPROVAL_ROLE ( '' ) ;
#7003 = LINE ( 'NONE', #6068, #10716 ) ;
#7004 = ORIENTED_EDGE ( 'NONE', *, *, #5550, .T. ) ;
#7005 = VECTOR ( 'NONE', #15062, 1000.000000000000000 ) ;
#7006 = CARTESIAN_POINT ( 'NONE',  ( 2.298097038856278029, 7.124999999999999112, -5.798097038856279362 ) ) ;
#7007 = CARTESIAN_POINT ( 'NONE',  ( -4.592425496802573972E-16, 8.999999999999998224, -7.250000000000000000 ) ) ;
#7008 = CARTESIAN_POINT ( 'NONE',  ( 30.32986759126112730, 0.000000000000000000, 43.04214087805580391 ) ) ;
#7009 = CARTESIAN_POINT ( 'NONE',  ( -64.01558189167985802, 12.98106818083026681, -201.5482190537578902 ) ) ;
#7010 = CARTESIAN_POINT ( 'NONE',  ( 0.7195110302018304926, 4.291397982413823975, -138.3948393236508139 ) ) ;
#7011 = CARTESIAN_POINT ( 'NONE',  ( 2.298097038856279362, 0.3750000000000001110, -1.201902961143720860 ) ) ;
#7012 = VECTOR ( 'NONE', #6517, 1000.000000000000000 ) ;
#7013 = CARTESIAN_POINT ( 'NONE',  ( -2.691470893477765802, 4.336808689942017736E-16, -114.7599528768529495 ) ) ;
#7014 = DATE_AND_TIME ( #9561, #1040 ) ;
#7015 = CARTESIAN_POINT ( 'NONE',  ( 3.249999999999999556, 14.75000000000000178, -3.500000000000000000 ) ) ;
#7016 = CARTESIAN_POINT ( 'NONE',  ( -0.3766621274091715987, -0.2500000000000000000, 0.1491815183709511716 ) ) ;
#7017 = ORIENTED_EDGE ( 'NONE', *, *, #11652, .T. ) ;
#7018 = CARTESIAN_POINT ( 'NONE',  ( -29.26478672069536913, 4.000000000000235367, -202.3577337911947609 ) ) ;
#7019 = CARTESIAN_POINT ( 'NONE',  ( -1.346194077712558945, 1.062500000000000222, -0.2500000000000002220 ) ) ;
#7020 = CARTESIAN_POINT ( 'NONE',  ( -6.683304552674627530, 4.336808689942017736E-16, -104.1296019027812179 ) ) ;
#7021 = CARTESIAN_POINT ( 'NONE',  ( -1.346194077712558945, 8.562500000000000000, -0.2500000000000002220 ) ) ;
#7022 = VERTEX_POINT ( 'NONE', #3516 ) ;
#7023 = CARTESIAN_POINT ( 'NONE',  ( -6.708306528330162166, 9.999999999999998224, -119.6038561065980446 ) ) ;
#7024 = CARTESIAN_POINT ( 'NONE',  ( -25.11906781955738310, 0.000000000000000000, -198.9681998140721078 ) ) ;
#7025 = CARTESIAN_POINT ( 'NONE',  ( 6.209053725235345489, 13.78527700952190571, 3.560231868336729111 ) ) ;
#7026 = EDGE_CURVE ( 'NONE', #7860, #2992, #3597, .T. ) ;
#7027 = CARTESIAN_POINT ( 'NONE',  ( -2.298097038856278473, 1.125000000000000222, -1.201902961143720416 ) ) ;
#7028 = CARTESIAN_POINT ( 'NONE',  ( 3.249999999999998224, 13.18750000000000000, -4.846194077712561388 ) ) ;
#7029 = CARTESIAN_POINT ( 'NONE',  ( 3.391286578035700217, 8.673617379884033500E-16, -107.3770126362747419 ) ) ;
#7030 = CARTESIAN_POINT ( 'NONE',  ( -2.651650429449552870, 1.625000000000000000, -0.8483495705504463524 ) ) ;
#7031 = PLANE ( 'NONE',  #6188 ) ;
#7032 = CARTESIAN_POINT ( 'NONE',  ( 1.004809442601929836, 5.333333333333333925, -139.4752805618705622 ) ) ;
#7033 = CARTESIAN_POINT ( 'NONE',  ( -2.117817860744609426, 2.099999999999999645, 38.45417591392908463 ) ) ;
#7034 = CARTESIAN_POINT ( 'NONE',  ( -3.249999999999999556, 11.18749999999999822, -2.153805922287440833 ) ) ;
#7035 = CARTESIAN_POINT ( 'NONE',  ( 2.700353918670075792, 15.00000000003971223, -24.42150847873306319 ) ) ;
#7036 = CARTESIAN_POINT ( 'NONE',  ( 7.353370788917347411, 9.030812432661041239E-12, -111.8370434415751475 ) ) ;
#7037 = ORIENTED_EDGE ( 'NONE', *, *, #13014, .F. ) ;
#7038 = ORIENTED_EDGE ( 'NONE', *, *, #12446, .F. ) ;
#7039 = CARTESIAN_POINT ( 'NONE',  ( 8.360009203849724457, 12.50000000000000000, -115.0372004058238389 ) ) ;
#7040 = CARTESIAN_POINT ( 'NONE',  ( 2.651650429449553759, 3.875000000000000000, -0.8483495705504471296 ) ) ;
#7041 = CARTESIAN_POINT ( 'NONE',  ( -3.750000000000000000, 2.687500000000000888, -1.946699141100893149 ) ) ;
#7042 = CARTESIAN_POINT ( 'NONE',  ( 3.136841903360914952, 15.00000000000000711, -104.4936450199714812 ) ) ;
#7043 = VERTEX_POINT ( 'NONE', #4605 ) ;
#7044 = EDGE_CURVE ( 'NONE', #7693, #4358, #7755, .T. ) ;
#7045 =( BOUNDED_SURFACE ( )  B_SPLINE_SURFACE ( 3, 2, ( 
 ( #8414, #2632, #7334 ),
 ( #12287, #1697, #6178 ),
 ( #313, #8651, #1394 ),
 ( #545, #9746, #3706 ),
 ( #5104, #228, #3871 ),
 ( #7259, #9894, #13147 ),
 ( #4029, #2556, #12045 ),
 ( #5027, #6097, #14474 ),
 ( #10812, #6261, #4944 ),
 ( #9659, #13305, #2707 ),
 ( #13385, #12132, #1548 ),
 ( #10978, #395, #8733 ),
 ( #2790, #7492, #13466 ),
 ( #12211, #1626, #6339 ),
 ( #11053, #12588, #699 ),
 ( #11278, #2081, #12438 ),
 ( #1778, #13616, #5404 ),
 ( #14782, #10201, #6566 ) ),
 .UNSPECIFIED., .F., .F., .T. ) 
 B_SPLINE_SURFACE_WITH_KNOTS ( ( 4, 2, 2, 2, 2, 2, 2, 2, 4 ),
 ( 3, 3 ),
 ( 0.000000000000000000, 0.0007443649107546155674, 0.001488729821509231135, 0.002233094732263846485, 0.002977459643018462269, 0.003721824553773077620, 0.004466189464527692971, 0.005210554375282308755, 0.005954919286036924539 ),
 ( 0.000000000000000000, 1.000000000000000000 ),
 .UNSPECIFIED. ) 
 GEOMETRIC_REPRESENTATION_ITEM ( )  RATIONAL_B_SPLINE_SURFACE ( (
 ( 1.000000000000000000, 0.7071067811865460184, 1.000000000000000000),
 ( 1.000000000000000000, 0.6972119573952525462, 1.000000000000000000),
 ( 1.000000000000000000, 0.6862390331242504971, 1.000000000000000000),
 ( 1.000000000000000000, 0.6643322149117374398, 1.000000000000000000),
 ( 1.000000000000000000, 0.6532829606877528228, 1.000000000000000000),
 ( 1.000000000000000000, 0.6342007904900059945, 1.000000000000000000),
 ( 1.000000000000000000, 0.6261622867538135795, 1.000000000000000000),
 ( 1.000000000000000000, 0.6149761046979081991, 1.000000000000000000),
 ( 1.000000000000000000, 0.6119284778760083476, 1.000000000000000000),
 ( 1.000000000000000000, 0.6119088882623058279, 1.000000000000000000),
 ( 1.000000000000000000, 0.6148452971779246878, 1.000000000000000000),
 ( 1.000000000000000000, 0.6260511252444348473, 1.000000000000000000),
 ( 1.000000000000000000, 0.6341360142629537400, 1.000000000000000000),
 ( 1.000000000000000000, 0.6531158155794938303, 1.000000000000000000),
 ( 1.000000000000000000, 0.6641411866188042801, 1.000000000000000000),
 ( 1.000000000000000000, 0.6862036393175137139, 1.000000000000000000),
 ( 1.000000000000000000, 0.6972164765192375713, 1.000000000000000000),
 ( 1.000000000000000000, 0.7071067811865491270, 1.000000000000000000) ) ) 
 REPRESENTATION_ITEM ( '' )  SURFACE ( )  );
#7046 = CARTESIAN_POINT ( 'NONE',  ( 1.346194077712558279, 1.062500000000000444, -6.750000000000000888 ) ) ;
#7047 = EDGE_CURVE ( 'NONE', #881, #16, #15282, .T. ) ;
#7048 = DIRECTION ( 'NONE',  ( 1.000000000000000000, 0.000000000000000000, 0.000000000000000000 ) ) ;
#7049 = CARTESIAN_POINT ( 'NONE',  ( 4.184249394548969825, 8.673617379884035472E-16, -108.7922730648138696 ) ) ;
#7050 = CARTESIAN_POINT ( 'NONE',  ( -3.980102097228897245E-16, 3.500000000000000000, -6.749999999999999112 ) ) ;
#7051 = DIRECTION ( 'NONE',  ( -0.04581719776170027625, 0.000000000000000000, 0.9989498407774363153 ) ) ;
#7052 = CARTESIAN_POINT ( 'NONE',  ( 0.7644969749118040170, 5.000000000000000000, -138.4027240657576101 ) ) ;
#7053 = ORIENTED_EDGE ( 'NONE', *, *, #9281, .T. ) ;
#7054 = CYLINDRICAL_SURFACE ( 'NONE', #11120, 5.000000000000000000 ) ;
#7055 = CARTESIAN_POINT ( 'NONE',  ( 0.000000000000000000, 14.00000000000000000, -0.2500000000000002220 ) ) ;
#7056 = ORIENTED_EDGE ( 'NONE', *, *, #9712, .T. ) ;
#7057 = ORIENTED_EDGE ( 'NONE', *, *, #1240, .T. ) ;
#7058 = CARTESIAN_POINT ( 'NONE',  ( 4.869735923794942245, 2.331468351711882200E-16, 48.16793894843318924 ) ) ;
#7059 = CARTESIAN_POINT ( 'NONE',  ( 2.651650429449554203, 7.375000000000000000, -0.8483495705504471296 ) ) ;
#7060 = CARTESIAN_POINT ( 'NONE',  ( 0.000000000000000000, 8.500000000000000000, -0.2500000000000002220 ) ) ;
#7061 = ORIENTED_EDGE ( 'NONE', *, *, #2156, .T. ) ;
#7062 = CARTESIAN_POINT ( 'NONE',  ( -2.424117393064570525, 15.00000000000080824, -107.6599666632758527 ) ) ;
#7063 = CARTESIAN_POINT ( 'NONE',  ( -1.346194077712559389, 4.062500000000000000, -0.2500000000000002220 ) ) ;
#7064 = EDGE_CURVE ( 'NONE', #15130, #1352, #2514, .T. ) ;
#7065 = CARTESIAN_POINT ( 'NONE',  ( 3.749999999999999112, 10.81250000000000178, -1.946699141100892039 ) ) ;
#7066 = CARTESIAN_POINT ( 'NONE',  ( -7.011153618232597751, 0.01937457977056467398, -104.1953234560537425 ) ) ;
#7067 = CARTESIAN_POINT ( 'NONE',  ( -1.258237567103696941, -6.071532165918825619E-15, -125.0317944887032979 ) ) ;
#7068 = CARTESIAN_POINT ( 'NONE',  ( 7.484376272073578029, 15.00000000000000000, -107.6919899575756006 ) ) ;
#7069 = COORDINATED_UNIVERSAL_TIME_OFFSET ( 0, 0, .AHEAD. ) ;
#7070 = CARTESIAN_POINT ( 'NONE',  ( -50.03010188096263988, 15.00000000000000000, -151.4930374104633870 ) ) ;
#7071 = VERTEX_POINT ( 'NONE', #13968 ) ;
#7072 = CARTESIAN_POINT ( 'NONE',  ( 5.376486659670671742, 1.020558061026469510, -45.55632290616389923 ) ) ;
#7073 = CARTESIAN_POINT ( 'NONE',  ( -4.592425496802573972E-16, 13.00000000000000000, -7.250000000000000000 ) ) ;
#7074 = PLANE ( 'NONE',  #4465 ) ;
#7075 = CARTESIAN_POINT ( 'NONE',  ( -66.00101815392289950, 14.98497452121014994, -193.2201357435544082 ) ) ;
#7076 = CARTESIAN_POINT ( 'NONE',  ( 30.96695154071790412, 8.773889247172311556, -44.17511166891541308 ) ) ;
#7077 = CARTESIAN_POINT ( 'NONE',  ( 0.000000000000000000, 1.500000000000000222, -0.2500000000000002220 ) ) ;
#7078 = CARTESIAN_POINT ( 'NONE',  ( 9.292954653762432571, 0.9864195427336619471, -105.8157378072028365 ) ) ;
#7079 = PERSON_AND_ORGANIZATION_ROLE ( 'design_owner' ) ;
#7080 = CARTESIAN_POINT ( 'NONE',  ( 4.856804767890306351, 14.90536770052033866, -1.840041787218210878 ) ) ;
#7081 = CARTESIAN_POINT ( 'NONE',  ( 4.286263797015736595E-16, 5.000000000000000000, 3.500000000000000000 ) ) ;
#7082 = ORIENTED_EDGE ( 'NONE', *, *, #1537, .T. ) ;
#7083 = CARTESIAN_POINT ( 'NONE',  ( -2.298097038856278473, 1.125000000000000222, -1.201902961143720416 ) ) ;
#7084 = CARTESIAN_POINT ( 'NONE',  ( -60.56192452144297533, 9.999999999999998224, -187.5450233986887554 ) ) ;
#7085 = AXIS2_PLACEMENT_3D ( 'NONE', #5784, #3466, #14940 ) ;
#7086 = CARTESIAN_POINT ( 'NONE',  ( 0.000000000000000000, 5.500000000000000888, -0.2500000000000002220 ) ) ;
#7087 = ORIENTED_EDGE ( 'NONE', *, *, #1771, .F. ) ;
#7088 = CARTESIAN_POINT ( 'NONE',  ( -7.119867912863494297, 15.00000000000182077, -107.3464651433156121 ) ) ;
#7089 = CARTESIAN_POINT ( 'NONE',  ( -28.38930394846591909, 15.00000000000000000, -151.9126338648069918 ) ) ;
#7090 = CARTESIAN_POINT ( 'NONE',  ( -19.94423925787078034, 15.00000000000000000, -150.2885610952392881 ) ) ;
#7091 = CARTESIAN_POINT ( 'NONE',  ( 16.50094977371536231, 8.749999999999998224, -91.72275351520976017 ) ) ;
#7092 = CARTESIAN_POINT ( 'NONE',  ( 3.749999999999999112, 3.312500000000000000, -1.946699141100893149 ) ) ;
#7093 = CARTESIAN_POINT ( 'NONE',  ( -3.750000000000000000, 4.187500000000000000, -1.946699141100892927 ) ) ;
#7094 = CARTESIAN_POINT ( 'NONE',  ( 4.018210755790066813, 8.673617379884037444E-16, -105.8455740756232473 ) ) ;
#7095 = CARTESIAN_POINT ( 'NONE',  ( -4.592425496802573972E-16, 4.000000000000000888, -7.250000000000000000 ) ) ;
#7096 = CARTESIAN_POINT ( 'NONE',  ( 0.7644969749118040170, 5.000000000000000000, -138.4027240657576101 ) ) ;
#7097 = FACE_OUTER_BOUND ( 'NONE', #3347, .T. ) ;
#7098 = DIRECTION ( 'NONE',  ( 0.05964429961207245307, 0.000000000000000000, 0.9982196940171964572 ) ) ;
#7099 = CARTESIAN_POINT ( 'NONE',  ( 3.249999999999999556, 10.75000000000000000, -3.500000000000000000 ) ) ;
#7100 = EDGE_CURVE ( 'NONE', #688, #6640, #6463, .T. ) ;
#7101 = CARTESIAN_POINT ( 'NONE',  ( 23.12860366745965734, 0.000000000000000000, 67.62772795920155033 ) ) ;
#7102 = CARTESIAN_POINT ( 'NONE',  ( -1.346194077712559389, 12.06250000000000000, -0.2500000000000002220 ) ) ;
#7103 = CARTESIAN_POINT ( 'NONE',  ( 8.595858757291594543, 5.000000000000000888, -113.5677547687719624 ) ) ;
#7104 = ORIENTED_EDGE ( 'NONE', *, *, #9325, .T. ) ;
#7105 = ORIENTED_EDGE ( 'NONE', *, *, #9905, .T. ) ;
#7106 = CARTESIAN_POINT ( 'NONE',  ( -7.218906882678753689, 2.645201729013087203E-12, -107.2047439206050399 ) ) ;
#7107 = DIRECTION ( 'NONE',  ( 0.000000000000000000, -0.000000000000000000, -1.000000000000000000 ) ) ;
#7108 = CARTESIAN_POINT ( 'NONE',  ( -1.553300858899106629, 6.062500000000000000, 0.2500000000000002220 ) ) ;
#7109 = CARTESIAN_POINT ( 'NONE',  ( -3.750000000000000000, 5.687500000000000888, -1.946699141100893149 ) ) ;
#7110 = CARTESIAN_POINT ( 'NONE',  ( -17.43524186648903296, 0.7231160150647996110, -130.1141235465726425 ) ) ;
#7111 = ORIENTED_EDGE ( 'NONE', *, *, #997, .T. ) ;
#7112 = CARTESIAN_POINT ( 'NONE',  ( 0.000000000000000000, 0.4999999999999999445, -0.2500000000000002220 ) ) ;
#7113 = CARTESIAN_POINT ( 'NONE',  ( -49.70557948973527118, 9.999999999999998224, -143.6055563701139306 ) ) ;
#7114 = CARTESIAN_POINT ( 'NONE',  ( 5.228075279701640099, 1.000000000000000000, -165.7939279834373849 ) ) ;
#7115 = MANIFOLD_SOLID_BREP ( 'Saliente-Extruir1', #14998 ) ;
#7116 = CARTESIAN_POINT ( 'NONE',  ( 0.000000000000000000, 5.000000000000000000, -0.2500000000000002220 ) ) ;
#7117 = FACE_OUTER_BOUND ( 'NONE', #9269, .T. ) ;
#7118 = CARTESIAN_POINT ( 'NONE',  ( 20.97724033793567600, 8.673617379884035472E-16, -139.0817640602418805 ) ) ;
#7119 = ORIENTED_EDGE ( 'NONE', *, *, #1205, .F. ) ;
#7120 = EDGE_CURVE ( 'NONE', #13371, #6929, #10850, .T. ) ;
#7121 = FACE_OUTER_BOUND ( 'NONE', #3165, .T. ) ;
#7122 = CARTESIAN_POINT ( 'NONE',  ( 0.4711736884522539359, 9.999999999999998224, 5.336993082470237404 ) ) ;
#7123 = ORIENTED_EDGE ( 'NONE', *, *, #4389, .T. ) ;
#7124 = VERTEX_POINT ( 'NONE', #3828 ) ;
#7125 = CARTESIAN_POINT ( 'NONE',  ( -26.77342622694935059, 4.000000000000000000, -207.3649691462522924 ) ) ;
#7126 =( BOUNDED_CURVE ( )  B_SPLINE_CURVE ( 3, ( #7487, #14986, #464, #12570 ),
 .UNSPECIFIED., .F., .F. ) 
 B_SPLINE_CURVE_WITH_KNOTS ( ( 4, 4 ),
 ( 3.460670697713912336, 3.568893446053258867 ),
 .UNSPECIFIED. ) 
 CURVE ( )  GEOMETRIC_REPRESENTATION_ITEM ( )  RATIONAL_B_SPLINE_CURVE ( ( 1.000000000000000000, 0.9990242245225531281, 0.9990242245225531281, 1.000000000000000000 ) ) 
 REPRESENTATION_ITEM ( '' )  );
#7127 = CARTESIAN_POINT ( 'NONE',  ( -3.750000000000000000, 6.687500000000000888, -1.946699141100893149 ) ) ;
#7128 = CARTESIAN_POINT ( 'NONE',  ( 3.249999999999998224, 5.187500000000001776, -4.846194077712561388 ) ) ;
#7129 = ORIENTED_EDGE ( 'NONE', *, *, #10627, .T. ) ;
#7130 = CARTESIAN_POINT ( 'NONE',  ( 6.222982598701390700, 13.98190557557194502, 3.317519625265672456 ) ) ;
#7131 = CARTESIAN_POINT ( 'NONE',  ( -2.298097038856278473, 4.125000000000000000, -1.201902961143720416 ) ) ;
#7132 = APPROVAL_PERSON_ORGANIZATION ( #7137, #668, #9175 ) ;
#7133 = VECTOR ( 'NONE', #1654, 1000.000000000000000 ) ;
#7134 = CARTESIAN_POINT ( 'NONE',  ( -5.208811060977222240, 2.500000000000000888, -111.9226923171489432 ) ) ;
#7135 = CARTESIAN_POINT ( 'NONE',  ( 11.30894640059546852, 0.7539637541287584899, -164.8338407189809232 ) ) ;
#7136 = CARTESIAN_POINT ( 'NONE',  ( 9.697783895759762629, 15.00000000000000000, -124.7881275717043650 ) ) ;
#7137 = PERSON_AND_ORGANIZATION ( #3176, #3020 ) ;
#7138 = DIRECTION ( 'NONE',  ( 0.000000000000000000, 0.000000000000000000, -1.000000000000000000 ) ) ;
#7139 = EDGE_CURVE ( 'NONE', #9693, #6034, #6265, .T. ) ;
#7140 = EDGE_CURVE ( 'NONE', #2776, #6060, #1, .T. ) ;
#7141 = LOCAL_TIME ( 12, 28, 20.00000000000000000, #14106 ) ;
#7142 = ORIENTED_EDGE ( 'NONE', *, *, #10732, .T. ) ;
#7143 = AXIS2_PLACEMENT_3D ( 'NONE', #14025, #817, #5520 ) ;
#7144 = CARTESIAN_POINT ( 'NONE',  ( 9.458437899194636955, 1.020558061026469510, -40.77697206847473410 ) ) ;
#7145 = CARTESIAN_POINT ( 'NONE',  ( 3.749999999999999112, 13.31250000000000178, -1.946699141100893149 ) ) ;
#7146 = PLANE ( 'NONE',  #4716 ) ;
#7147 = VECTOR ( 'NONE', #7792, 1000.000000000000000 ) ;
#7148 = CARTESIAN_POINT ( 'NONE',  ( -63.24235068824187067, 10.57596889784981720, -203.5428763147797611 ) ) ;
#7149 = DIRECTION ( 'NONE',  ( 0.000000000000000000, 0.000000000000000000, 1.000000000000000000 ) ) ;
#7150 = CARTESIAN_POINT ( 'NONE',  ( 2.298097038856279362, 4.375000000000000888, -1.201902961143720860 ) ) ;
#7151 = AXIS2_PLACEMENT_3D ( 'NONE', #8966, #6725, #785 ) ;
#7152 = CARTESIAN_POINT ( 'NONE',  ( 9.025311242897139152, 0.8923617020100302888, -106.1611430900688191 ) ) ;
#7153 = VECTOR ( 'NONE', #5519, 1000.000000000000227 ) ;
#7154 = DATE_AND_TIME ( #3540, #2036 ) ;
#7155 = AXIS2_PLACEMENT_3D ( 'NONE', #382, #14534, #13675 ) ;
#7156 = CARTESIAN_POINT ( 'NONE',  ( 0.7552767017137625993, 15.00000000000000178, -110.7727649483667989 ) ) ;
#7157 = DIRECTION ( 'NONE',  ( -0.000000000000000000, -1.000000000000000000, -0.000000000000000000 ) ) ;
#7158 = ORIENTED_EDGE ( 'NONE', *, *, #13203, .F. ) ;
#7159 = CARTESIAN_POINT ( 'NONE',  ( 8.251486519976570122, 2.457945381532850249, 2.437901666522639399 ) ) ;
#7160 = CARTESIAN_POINT ( 'NONE',  ( -3.249999999999999556, 3.312500000000000000, -4.846194077712557835 ) ) ;
#7161 = DIRECTION ( 'NONE',  ( -0.000000000000000000, -1.000000000000000000, -0.000000000000000000 ) ) ;
#7162 = AXIS2_PLACEMENT_3D ( 'NONE', #11171, #11399, #2981 ) ;
#7163 = CARTESIAN_POINT ( 'NONE',  ( 3.249999999999998224, 7.312500000000001776, -2.153805922287439945 ) ) ;
#7164 = ORIENTED_EDGE ( 'NONE', *, *, #6697, .F. ) ;
#7165 = CARTESIAN_POINT ( 'NONE',  ( -0.4878245559413970089, 15.00000000000000000, -109.9489936375345280 ) ) ;
#7166 = CARTESIAN_POINT ( 'NONE',  ( 0.7827419278469371910, 12.28707364804876612, 2.610748976233180585 ) ) ;
#7167 = CARTESIAN_POINT ( 'NONE',  ( 10.01939027896081669, 9.999999999999998224, -127.6977514918621637 ) ) ;
#7168 = AXIS2_PLACEMENT_3D ( 'NONE', #4127, #7967, #4497 ) ;
#7169 = CARTESIAN_POINT ( 'NONE',  ( -2.298097038856278918, 2.375000000000000000, -5.798097038856277585 ) ) ;
#7170 = CARTESIAN_POINT ( 'NONE',  ( -3.750000000000000000, 0.8124999999999997780, -5.053300858899105741 ) ) ;
#7171 = CARTESIAN_POINT ( 'NONE',  ( -4.592425496802573972E-16, 6.500000000000000888, -7.249999999999999112 ) ) ;
#7172 = CARTESIAN_POINT ( 'NONE',  ( 3.872594309009199876, 8.673617379884035472E-16, -106.2339216993545818 ) ) ;
#7173 = CARTESIAN_POINT ( 'NONE',  ( -2.651650429449553314, 7.874999999999999112, -6.151650429449552426 ) ) ;
#7174 = CARTESIAN_POINT ( 'NONE',  ( 2.957952336870751875, 14.53460293439382767, 0.6370940153772954861 ) ) ;
#7175 = CARTESIAN_POINT ( 'NONE',  ( 0.000000000000000000, 1.530808498934191509E-17, 0.000000000000000000 ) ) ;
#7176 = CARTESIAN_POINT ( 'NONE',  ( -8.814455821404541425, 1.837399608813588214, -105.4684601932094665 ) ) ;
#7177 = CARTESIAN_POINT ( 'NONE',  ( 3.717577911061872076, 8.673617379884035472E-16, -143.6771719914432595 ) ) ;
#7178 = CARTESIAN_POINT ( 'NONE',  ( 3.249999999999999112, 13.81250000000000000, -2.153805922287439945 ) ) ;
#7179 = CARTESIAN_POINT ( 'NONE',  ( -5.397979047513929984, 14.84615269367921719, -103.5376357543976980 ) ) ;
#7180 = CARTESIAN_POINT ( 'NONE',  ( -63.23328683196935174, 10.53727328510970551, -203.5631487748948700 ) ) ;
#7181 = ORIENTED_EDGE ( 'NONE', *, *, #14293, .F. ) ;
#7182 = CARTESIAN_POINT ( 'NONE',  ( 2.651650429449554203, 8.375000000000000000, -0.8483495705504471296 ) ) ;
#7183 = VERTEX_POINT ( 'NONE', #14663 ) ;
#7184 = CARTESIAN_POINT ( 'NONE',  ( -5.137754182254912649, 2.500000000000000444, -114.0283549521523696 ) ) ;
#7185 = CARTESIAN_POINT ( 'NONE',  ( -16.63253413790094726, 3.999999999999409361, -194.7535182948206511 ) ) ;
#7186 = CARTESIAN_POINT ( 'NONE',  ( -3.750000000000000000, 4.250000000000000000, -3.499999999999999112 ) ) ;
#7187 = CARTESIAN_POINT ( 'NONE',  ( 3.749999999999999556, 2.249999999999999556, -3.500000000000000444 ) ) ;
#7188 = FACE_OUTER_BOUND ( 'NONE', #10528, .T. ) ;
#7189 = ORIENTED_EDGE ( 'NONE', *, *, #8094, .F. ) ;
#7190 = CC_DESIGN_APPROVAL ( #13137, ( #8939 ) ) ;
#7191 = EDGE_CURVE ( 'NONE', #11845, #13038, #6136, .T. ) ;
#7192 = B_SPLINE_CURVE_WITH_KNOTS ( 'NONE', 3,
 ( #10035, #9026, #4169, #8873 ),
 .UNSPECIFIED., .F., .F.,
 ( 4, 4 ),
 ( 0.000000000000000000, 0.0003777938110651892596 ),
 .UNSPECIFIED. ) ;
#7193 = CARTESIAN_POINT ( 'NONE',  ( -7.409205697917243150, 0.9058721944443380858, -116.8849570398053572 ) ) ;
#7194 = CARTESIAN_POINT ( 'NONE',  ( -3.249999999999999112, 4.812500000000000000, -4.846194077712558723 ) ) ;
#7195 = CARTESIAN_POINT ( 'NONE',  ( -68.83694965420261269, 15.00000000000000000, -180.7144811896928331 ) ) ;
#7196 = CARTESIAN_POINT ( 'NONE',  ( 3.312745690571184287, 8.673617379884035472E-16, -113.0297142168659263 ) ) ;
#7197 =( NAMED_UNIT ( * ) SI_UNIT ( $, .STERADIAN. ) SOLID_ANGLE_UNIT ( ) );
#7198 = CARTESIAN_POINT ( 'NONE',  ( -3.249999999999999556, 6.187500000000000888, -2.153805922287440833 ) ) ;
#7199 = CARTESIAN_POINT ( 'NONE',  ( 20.38723710659885313, 7.321094445766561876, -31.17704722822712426 ) ) ;
#7200 = ITEM_DEFINED_TRANSFORMATION ( 'NONE', 'NONE', #12651,  #9419 ) ;
#7201 = CC_DESIGN_APPROVAL ( #10068, ( #2984 ) ) ;
#7202 = DIRECTION ( 'NONE',  ( 0.000000000000000000, 1.000000000000000000, 0.000000000000000000 ) ) ;
#7203 = CARTESIAN_POINT ( 'NONE',  ( 11.96422411991965618, 8.673617379884035472E-16, -131.4923627482014012 ) ) ;
#7204 = ORIENTED_EDGE ( 'NONE', *, *, #6737, .T. ) ;
#7205 = CARTESIAN_POINT ( 'NONE',  ( 0.01496453197139708223, 5.000000000000000000, 5.196130874293197088 ) ) ;
#7206 = CARTESIAN_POINT ( 'NONE',  ( -2.298097038856278918, 14.37500000000000000, -5.798097038856277585 ) ) ;
#7207 = ORIENTED_EDGE ( 'NONE', *, *, #8371, .T. ) ;
#7208 = ORIENTED_EDGE ( 'NONE', *, *, #9025, .F. ) ;
#7209 = CARTESIAN_POINT ( 'NONE',  ( -25.72020873159803855, 4.000000000000001776, -208.7304761312111623 ) ) ;
#7210 = CARTESIAN_POINT ( 'NONE',  ( -2.651650429449552870, 6.625000000000000888, -0.8483495705504463524 ) ) ;
#7211 = VECTOR ( 'NONE', #13479, 1000.000000000000000 ) ;
#7212 = CARTESIAN_POINT ( 'NONE',  ( 0.000000000000000000, 9.500000000000000000, -0.2500000000000002220 ) ) ;
#7213 = EDGE_LOOP ( 'NONE', ( #11808, #11111, #14578, #9378 ) ) ;
#7214 = EDGE_CURVE ( 'NONE', #12142, #8185, #10956, .T. ) ;
#7215 = CARTESIAN_POINT ( 'NONE',  ( 4.999999996894303855, 14.99999999999999822, -101.5775160893471138 ) ) ;
#7216 = CARTESIAN_POINT ( 'NONE',  ( 3.249999999999998668, 8.687500000000000000, -4.846194077712560500 ) ) ;
#7217 = EDGE_CURVE ( 'NONE', #8407, #3224, #9786, .T. ) ;
#7218 = CARTESIAN_POINT ( 'NONE',  ( -7.952046529484080750, 0.3056169037709979275, -104.3879148205416385 ) ) ;
#7219 = CARTESIAN_POINT ( 'NONE',  ( -53.86916490710522964, 10.00000000000000355, -170.7116325868586557 ) ) ;
#7220 = CARTESIAN_POINT ( 'NONE',  ( -49.62396416653276532, 15.00000000000000178, -157.5220014270338424 ) ) ;
#7221 = ADVANCED_BREP_SHAPE_REPRESENTATION ( '', ( #2311, #9419 ), #14368 ) ;
#7222 = CIRCLE ( 'NONE', #4760, 1.250000000000005107 ) ;
#7223 = APPROVAL_DATE_TIME ( #8616, #11573 ) ;
#7224 = CARTESIAN_POINT ( 'NONE',  ( -63.60348060676458459, 15.00000000000000000, -180.2685449772604045 ) ) ;
#7225 =( BOUNDED_SURFACE ( )  B_SPLINE_SURFACE ( 3, 2, ( 
 ( #4947, #9663, #11818 ),
 ( #14394, #14308, #3709 ),
 ( #14785, #13469, #2872 ),
 ( #3874, #6414, #12048 ),
 ( #8575, #316, #8812 ),
 ( #6266, #1783, #4182 ),
 ( #9749, #2635, #8738 ),
 ( #12290, #1700, #11056 ),
 ( #10900, #10981, #12214 ),
 ( #11132, #7497, #550 ),
 ( #5261, #13233, #473 ),
 ( #9973, #14711, #7337 ),
 ( #4111, #13542, #2941 ),
 ( #14634, #9822, #7571 ),
 ( #5188, #1469, #6181 ),
 ( #4032, #5032, #14477 ) ),
 .UNSPECIFIED., .F., .F., .F. ) 
 B_SPLINE_SURFACE_WITH_KNOTS ( ( 4, 2, 2, 2, 2, 2, 2, 4 ),
 ( 3, 3 ),
 ( -1.714383521174504596E-05, 0.001390813748932505714, 0.002094792541004631119, 0.002798771333076756525, 0.003502750125148881930, 0.004206728917221007336, 0.004910707709293133175, 0.005614686501365258146 ),
 ( 0.000000000000000000, 1.000000000000000000 ),
 .UNSPECIFIED. ) 
 GEOMETRIC_REPRESENTATION_ITEM ( )  RATIONAL_B_SPLINE_SURFACE ( (
 ( 1.000000000000000000, 1.000000000000000000, 1.000000000000000000),
 ( 1.000000000000000000, 1.000000047483659893, 1.000000000000000000),
 ( 1.000000000000000000, 0.9984278383163904813, 1.000000000000000000),
 ( 1.000000000000000000, 0.9939583932889539675, 1.000000000000000000),
 ( 1.000000000000000000, 0.9921436623915373954, 1.000000000000000000),
 ( 1.000000000000000000, 0.9880575292902304962, 1.000000000000000000),
 ( 1.000000000000000000, 0.9857791852598755122, 1.000000000000000000),
 ( 1.000000000000000000, 0.9809189248842778985, 1.000000000000000000),
 ( 1.000000000000000000, 0.9783729182749338893, 1.000000000000000000),
 ( 1.000000000000000000, 0.9733849987678442339, 1.000000000000000000),
 ( 1.000000000000000000, 0.9709255430829486500, 1.000000000000000000),
 ( 1.000000000000000000, 0.9663197370312965884, 1.000000000000000000),
 ( 1.000000000000000000, 0.9642109238660780957, 1.000000000000000000),
 ( 1.000000000000000000, 0.9606928177971931770, 1.000000000000000000),
 ( 1.000000000000000000, 0.9592645092514092697, 1.000000000000000000),
 ( 1.000000000000000000, 0.9582603755229887055, 1.000000000000000000) ) ) 
 REPRESENTATION_ITEM ( '' )  SURFACE ( )  );
#7226 = ORIENTED_EDGE ( 'NONE', *, *, #10165, .F. ) ;
#7227 = CC_DESIGN_DATE_AND_TIME_ASSIGNMENT ( #12180, #13197, ( #8377 ) ) ;
#7228 = CARTESIAN_POINT ( 'NONE',  ( -6.435381799839732686, 9.999999999999998224, -129.7490639376177626 ) ) ;
#7229 = VECTOR ( 'NONE', #11222, 1000.000000000000000 ) ;
#7230 = AXIS2_PLACEMENT_3D ( 'NONE', #11431, #7948, #5782 ) ;
#7231 = EDGE_CURVE ( 'NONE', #13718, #7952, #10220, .T. ) ;
#7232 = CARTESIAN_POINT ( 'NONE',  ( -2.651650429449552870, 14.87500000000000355, -6.151650429449552426 ) ) ;
#7233 = ADVANCED_FACE ( 'NONE', ( #352 ), #3747, .F. ) ;
#7234 = CARTESIAN_POINT ( 'NONE',  ( 1.004149434879655578, 5.000000000000000888, -139.4756852570866670 ) ) ;
#7235 = EDGE_CURVE ( 'NONE', #11957, #12332, #10457, .T. ) ;
#7236 = CARTESIAN_POINT ( 'NONE',  ( -67.59193506824016140, 10.78987469597949556, -204.3712682500590176 ) ) ;
#7237 = LINE ( 'NONE', #14283, #48 ) ;
#7238 = CARTESIAN_POINT ( 'NONE',  ( 2.298097038856279362, 3.375000000000000444, -1.201902961143720860 ) ) ;
#7239 = COORDINATED_UNIVERSAL_TIME_OFFSET ( 0, 0, .AHEAD. ) ;
#7240 = CARTESIAN_POINT ( 'NONE',  ( -4.203928810071235311, 14.18377006225550829, -125.2130536027671326 ) ) ;
#7241 = CIRCLE ( 'NONE', #604, 4.000000000000002665 ) ;
#7242 = DIRECTION ( 'NONE',  ( 1.000000000000000000, 0.000000000000000000, 0.000000000000000000 ) ) ;
#7243 = AXIS2_PLACEMENT_3D ( 'NONE', #6351, #12225, #5271 ) ;
#7244 = ORIENTED_EDGE ( 'NONE', *, *, #13596, .T. ) ;
#7245 = CARTESIAN_POINT ( 'NONE',  ( 6.214735144181003257, 0.3805900070242324573, 2.672050388266886678 ) ) ;
#7246 = CARTESIAN_POINT ( 'NONE',  ( 0.000000000000000000, 6.000000000000000000, -0.2500000000000002220 ) ) ;
#7247 = CARTESIAN_POINT ( 'NONE',  ( -69.15427381923166195, 9.999999999999998224, -182.3943105425532281 ) ) ;
#7248 = CARTESIAN_POINT ( 'NONE',  ( 1.346194077712558057, 12.56250000000000000, -6.750000000000000000 ) ) ;
#7249 = CARTESIAN_POINT ( 'NONE',  ( 2.298097038856279362, 6.375000000000000888, -1.201902961143720860 ) ) ;
#7250 = CARTESIAN_POINT ( 'NONE',  ( -5.541218901405696506, 15.00000000000060929, -110.3933575420945630 ) ) ;
#7251 = CARTESIAN_POINT ( 'NONE',  ( 2.088366663672936774, 13.96978715545234095, 1.558942282566567972 ) ) ;
#7252 = CARTESIAN_POINT ( 'NONE',  ( -14.37903708479884557, 14.99999999998933120, -152.3617959900740289 ) ) ;
#7253 = CARTESIAN_POINT ( 'NONE',  ( 2.298097038856278473, 2.625000000000000000, -5.798097038856279362 ) ) ;
#7254 = VECTOR ( 'NONE', #2299, 1000.000000000000114 ) ;
#7255 = CARTESIAN_POINT ( 'NONE',  ( 3.749999999999999556, 2.249999999999999556, -3.500000000000000444 ) ) ;
#7256 = EDGE_CURVE ( 'NONE', #5560, #6301, #13193, .T. ) ;
#7257 = CARTESIAN_POINT ( 'NONE',  ( -2.651650429449553314, 4.375000000000000000, -6.151650429449552426 ) ) ;
#7258 = CC_DESIGN_PERSON_AND_ORGANIZATION_ASSIGNMENT ( #13905, #13978, ( #8872 ) ) ;
#7259 = CARTESIAN_POINT ( 'NONE',  ( -3.517668735334777530, 10.45885036913166033, -46.62850106167113040 ) ) ;
#7260 = CARTESIAN_POINT ( 'NONE',  ( 1.553300858899109516, 6.437500000000000888, 0.2499999999999993616 ) ) ;
#7261 = CARTESIAN_POINT ( 'NONE',  ( 1.128730403528703130, 12.89415287894916595, 2.354358630481084624 ) ) ;
#7262 = DIRECTION ( 'NONE',  ( 0.9961255586397050887, -0.000000000000000000, -0.08794243244723005948 ) ) ;
#7263 = DIRECTION ( 'NONE',  ( 0.000000000000000000, -0.000000000000000000, 1.000000000000000000 ) ) ;
#7264 = CARTESIAN_POINT ( 'NONE',  ( -1.660557334999934076, 6.000000000000000000, -134.7186485042710729 ) ) ;
#7265 = CARTESIAN_POINT ( 'NONE',  ( -2.298097038856278918, 13.37500000000000000, -5.798097038856277585 ) ) ;
#7266 = CARTESIAN_POINT ( 'NONE',  ( 5.376722707423876813, 0.1900852925348768263, -0.2357307375419829543 ) ) ;
#7267 = DIRECTION ( 'NONE',  ( -0.05964429961207245307, 0.000000000000000000, -0.9982196940171964572 ) ) ;
#7268 = ORIENTED_EDGE ( 'NONE', *, *, #12215, .F. ) ;
#7269 = CARTESIAN_POINT ( 'NONE',  ( -2.651650429449552870, 10.62500000000000000, -0.8483495705504463524 ) ) ;
#7270 = ORIENTED_EDGE ( 'NONE', *, *, #4027, .F. ) ;
#7271 = CARTESIAN_POINT ( 'NONE',  ( -2.708352249312388160, 0.000000000000000000, -111.7675805608782014 ) ) ;
#7272 = CARTESIAN_POINT ( 'NONE',  ( 8.131300352726233527, -2.490287375297126626, -39.89901737624450107 ) ) ;
#7273 = CARTESIAN_POINT ( 'NONE',  ( -4.592425496802573972E-16, 10.50000000000000000, -7.249999999999999112 ) ) ;
#7274 = CARTESIAN_POINT ( 'NONE',  ( -2.651650429449552870, 4.875000000000000000, -6.151650429449552426 ) ) ;
#7275 = CARTESIAN_POINT ( 'NONE',  ( -18.09353981420494151, 5.000000000000000000, -129.3374956033359240 ) ) ;
#7276 = VERTEX_POINT ( 'NONE', #5139 ) ;
#7277 = CARTESIAN_POINT ( 'NONE',  ( -4.890501715614620437, -7.342728488552128110E-10, -117.3116236002538812 ) ) ;
#7278 = CARTESIAN_POINT ( 'NONE',  ( -2.298097038856278029, 4.624999999999999112, -1.201902961143720638 ) ) ;
#7279 = CARTESIAN_POINT ( 'NONE',  ( -69.93026694898610174, 15.00000000000057554, -195.9981257600232993 ) ) ;
#7280 = CARTESIAN_POINT ( 'NONE',  ( 3.843142374354968638, 8.673617379884033500E-16, -118.1836930616208008 ) ) ;
#7281 =( NAMED_UNIT ( * ) SI_UNIT ( $, .STERADIAN. ) SOLID_ANGLE_UNIT ( ) );
#7282 = CARTESIAN_POINT ( 'NONE',  ( 0.000000000000000000, 7.000000000000000000, -0.2500000000000002220 ) ) ;
#7283 = CARTESIAN_POINT ( 'NONE',  ( 5.000000000000001776, 15.00000000000000000, -1.663700395152567513 ) ) ;
#7284 = CARTESIAN_POINT ( 'NONE',  ( -6.027592498023851775, -1.580622335394386225E-12, -126.6584150166784326 ) ) ;
#7285 = CARTESIAN_POINT ( 'NONE',  ( 15.55318939603108852, 0.000000000000000000, -134.8337474659214479 ) ) ;
#7286 = ORIENTED_EDGE ( 'NONE', *, *, #10264, .T. ) ;
#7287 = DIRECTION ( 'NONE',  ( 0.000000000000000000, 0.000000000000000000, 1.000000000000000000 ) ) ;
#7288 = CARTESIAN_POINT ( 'NONE',  ( 1.346194077712560944, 13.93750000000000000, -0.2500000000000011102 ) ) ;
#7289 = VERTEX_POINT ( 'NONE', #9850 ) ;
#7290 = VERTEX_POINT ( 'NONE', #12247 ) ;
#7291 = CARTESIAN_POINT ( 'NONE',  ( 20.23335552821398409, 2.331468351713730107E-16, 65.44177069175029260 ) ) ;
#7292 = CARTESIAN_POINT ( 'NONE',  ( 3.749999999999999112, 13.31250000000000178, -1.946699141100893149 ) ) ;
#7293 = CARTESIAN_POINT ( 'NONE',  ( 3.249999999999998224, 6.187500000000001776, -4.846194077712561388 ) ) ;
#7294 = CARTESIAN_POINT ( 'NONE',  ( 3.249999999999998224, 11.31250000000000000, -2.153805922287439945 ) ) ;
#7295 = ORIENTED_EDGE ( 'NONE', *, *, #10937, .T. ) ;
#7296 = CARTESIAN_POINT ( 'NONE',  ( 0.2625675448779695720, 15.00000000000000000, 2.974107436473219401 ) ) ;
#7297 = CARTESIAN_POINT ( 'NONE',  ( 1.346194077712558057, 5.562500000000000000, -6.750000000000000000 ) ) ;
#7298 = CARTESIAN_POINT ( 'NONE',  ( -5.787114392161415211, 2.500000000000000444, -109.6579705534062157 ) ) ;
#7299 = CARTESIAN_POINT ( 'NONE',  ( -45.48687283825000804, 9.999999999999996447, -160.5939636279570948 ) ) ;
#7300 = CARTESIAN_POINT ( 'NONE',  ( -47.48189921986827500, 5.000000000000000888, -141.5723758807981483 ) ) ;
#7301 = COORDINATED_UNIVERSAL_TIME_OFFSET ( 0, 0, .AHEAD. ) ;
#7302 = EDGE_CURVE ( 'NONE', #1356, #6929, #605, .T. ) ;
#7303 = CARTESIAN_POINT ( 'NONE',  ( -24.89426390012435064, 2.111117962734504250, -207.5279892455088202 ) ) ;
#7304 = ORIENTED_EDGE ( 'NONE', *, *, #4783, .T. ) ;
#7305 = EDGE_CURVE ( 'NONE', #13571, #4732, #14217, .T. ) ;
#7306 = CARTESIAN_POINT ( 'NONE',  ( -3.249999999999999556, 9.312499999999998224, -4.846194077712557835 ) ) ;
#7307 = CARTESIAN_POINT ( 'NONE',  ( -2.298097038856278473, 2.125000000000000000, -1.201902961143720416 ) ) ;
#7308 = CARTESIAN_POINT ( 'NONE',  ( 3.554677347145018373, -2.225540348348185052E-17, 2.000000000000000000 ) ) ;
#7309 = CARTESIAN_POINT ( 'NONE',  ( -1.553300858899107073, 13.93750000000000000, -7.249999999999999112 ) ) ;
#7310 = PRODUCT_RELATED_PRODUCT_CATEGORY ( 'detail', '', ( #8304 ) ) ;
#7311 = CARTESIAN_POINT ( 'NONE',  ( -63.88640454979729100, 11.48906216229545585, -211.3082455422185433 ) ) ;
#7312 = DIRECTION ( 'NONE',  ( 0.000000000000000000, 0.000000000000000000, -1.000000000000000000 ) ) ;
#7313 = CARTESIAN_POINT ( 'NONE',  ( 2.298097038856278029, 2.125000000000000000, -5.798097038856279362 ) ) ;
#7314 = CARTESIAN_POINT ( 'NONE',  ( 10.68883385149069198, 14.16521505008430459, -106.2696755902874628 ) ) ;
#7315 = CALENDAR_DATE ( 2026, 8, 10 ) ;
#7316 = AXIS2_PLACEMENT_3D ( 'NONE', #15030, #14010, #10367 ) ;
#7317 = FACE_OUTER_BOUND ( 'NONE', #2728, .T. ) ;
#7318 = CARTESIAN_POINT ( 'NONE',  ( -0.01496453197141594735, 5.000000000000000000, -5.196130874293185542 ) ) ;
#7319 = EDGE_LOOP ( 'NONE', ( #12747, #8684, #8050, #1830 ) ) ;
#7320 = EDGE_CURVE ( 'NONE', #887, #10395, #1813, .T. ) ;
#7321 = CARTESIAN_POINT ( 'NONE',  ( 7.278275680548385473, 1.096586756138080432, 3.954380374118978914 ) ) ;
#7322 = CARTESIAN_POINT ( 'NONE',  ( -2.298097038856278918, 5.375000000000000000, -5.798097038856277585 ) ) ;
#7323 = EDGE_CURVE ( 'NONE', #6618, #5674, #3507, .T. ) ;
#7324 = CARTESIAN_POINT ( 'NONE',  ( -60.01991856039841622, 10.00000000000000000, -157.4353610330038009 ) ) ;
#7325 = CARTESIAN_POINT ( 'NONE',  ( 3.249999999999999112, 12.81250000000000000, -2.153805922287439945 ) ) ;
#7326 = CARTESIAN_POINT ( 'NONE',  ( -2.298097038856278029, 6.625000000000000888, -1.201902961143720638 ) ) ;
#7327 = CARTESIAN_POINT ( 'NONE',  ( -6.178332509794770999, 14.99999999999909051, -118.3334666057659916 ) ) ;
#7328 = DIRECTION ( 'NONE',  ( 0.000000000000000000, 1.000000000000000000, 0.000000000000000000 ) ) ;
#7329 = B_SPLINE_CURVE_WITH_KNOTS ( 'NONE', 3,
 ( #205, #11866, #9633, #4918, #14367, #130 ),
 .UNSPECIFIED., .F., .F.,
 ( 4, 2, 4 ),
 ( 0.000000000000000000, 0.004354769343283191457, 0.008709538686566382915 ),
 .UNSPECIFIED. ) ;
#7330 = CARTESIAN_POINT ( 'NONE',  ( -3.942526376278688627, 15.00000000000000000, -136.1336533158506370 ) ) ;
#7331 = DIRECTION ( 'NONE',  ( 0.000000000000000000, 0.000000000000000000, -1.000000000000000000 ) ) ;
#7332 = CARTESIAN_POINT ( 'NONE',  ( -3.750000000000000000, 1.812499999999999778, -5.053300858899105741 ) ) ;
#7333 = CARTESIAN_POINT ( 'NONE',  ( 2.651650429449553759, 3.875000000000000000, -0.8483495705504471296 ) ) ;
#7334 = CARTESIAN_POINT ( 'NONE',  ( -4.254413237569943718, 9.999999999999998224, -48.18981741835666099 ) ) ;
#7335 = CARTESIAN_POINT ( 'NONE',  ( -3.750000000000000000, 5.687500000000000888, -1.946699141100893149 ) ) ;
#7336 = CARTESIAN_POINT ( 'NONE',  ( 3.700411912290352490, 12.62857015470723177, 4.325284914432235617 ) ) ;
#7337 = CARTESIAN_POINT ( 'NONE',  ( 12.74513938997514195, 2.668544226154935028, -165.8867193072528323 ) ) ;
#7338 = CARTESIAN_POINT ( 'NONE',  ( -8.338108546337810623, 0.8313257340310024057, -105.1551276366440248 ) ) ;
#7339 = CARTESIAN_POINT ( 'NONE',  ( 1.346194077712560944, 10.93750000000000000, -0.2500000000000010547 ) ) ;
#7340 = CARTESIAN_POINT ( 'NONE',  ( 2.850044070969222076, 9.999999999999998224, -103.0233998225063345 ) ) ;
#7341 = CARTESIAN_POINT ( 'NONE',  ( 6.387831235576543421, 4.907497138154600617E-16, -139.1888589629733133 ) ) ;
#7342 = ADVANCED_FACE ( 'NONE', ( #12701, #5585 ), #11388, .T. ) ;
#7343 = CARTESIAN_POINT ( 'NONE',  ( -23.68520063642048257, 8.673617379884034486E-16, -180.0072976255214883 ) ) ;
#7344 = CARTESIAN_POINT ( 'NONE',  ( 0.3766621274091715987, 0.2956834184403337451, -6.863050255469942407 ) ) ;
#7345 = ORIENTED_EDGE ( 'NONE', *, *, #14826, .T. ) ;
#7346 = CARTESIAN_POINT ( 'NONE',  ( -2.651650429449552870, 9.624999999999998224, -0.8483495705504463524 ) ) ;
#7347 = VERTEX_POINT ( 'NONE', #5435 ) ;
#7348 = CARTESIAN_POINT ( 'NONE',  ( -5.346294835628299325, 2.500000000000000444, -111.0961406517456993 ) ) ;
#7349 = CARTESIAN_POINT ( 'NONE',  ( -19.98060382417750702, 2.666703424072985286E-12, -198.2865109825601735 ) ) ;
#7350 = CARTESIAN_POINT ( 'NONE',  ( 1.553300858899108849, 7.937500000000000888, 0.2499999999999993616 ) ) ;
#7351 = CARTESIAN_POINT ( 'NONE',  ( 2.651650429449553314, 9.374999999999998224, -0.8483495705504476847 ) ) ;
#7352 = CARTESIAN_POINT ( 'NONE',  ( 7.788671722263528885, 7.321094445766561876, -20.36947622874119546 ) ) ;
#7353 = ORIENTED_EDGE ( 'NONE', *, *, #2711, .F. ) ;
#7354 = CARTESIAN_POINT ( 'NONE',  ( -7.653276971142799923, 1.000796838352786100, -116.4876868865816704 ) ) ;
#7355 = CARTESIAN_POINT ( 'NONE',  ( -2.298097038856279362, 5.875000000000000888, -5.798097038856278473 ) ) ;
#7356 = CARTESIAN_POINT ( 'NONE',  ( -3.749999999999999556, 11.31249999999999822, -5.053300858899104853 ) ) ;
#7357 = CARTESIAN_POINT ( 'NONE',  ( -69.93026694944160226, 9.999999999999998224, -195.9981257600672677 ) ) ;
#7358 = CARTESIAN_POINT ( 'NONE',  ( 26.71007981443199952, 15.00000000000000000, -136.8791680534710054 ) ) ;
#7359 = DIRECTION ( 'NONE',  ( 0.000000000000000000, 0.000000000000000000, 1.000000000000000000 ) ) ;
#7360 = CARTESIAN_POINT ( 'NONE',  ( -3.249999999999999556, 9.250000000000000000, -3.499999999999999556 ) ) ;
#7361 = DATE_TIME_ROLE ( 'classification_date' ) ;
#7362 = CARTESIAN_POINT ( 'NONE',  ( 1.101407610004066395, 4.336808689942017736E-15, -129.3199319192200392 ) ) ;
#7363 = CARTESIAN_POINT ( 'NONE',  ( 9.719609032807245086, 1.952651032223853462E-12, -108.8314952392251058 ) ) ;
#7364 = ORIENTED_EDGE ( 'NONE', *, *, #7971, .F. ) ;
#7365 = CARTESIAN_POINT ( 'NONE',  ( -1.346194077712559167, 13.43750000000000000, -6.749999999999999112 ) ) ;
#7366 = ORIENTED_EDGE ( 'NONE', *, *, #1022, .F. ) ;
#7367 = ORIENTED_EDGE ( 'NONE', *, *, #665, .T. ) ;
#7368 = DIRECTION ( 'NONE',  ( -0.4304374328763156954, 0.000000000000000000, 0.9026204165532970558 ) ) ;
#7369 = CARTESIAN_POINT ( 'NONE',  ( -3.750000000000000000, 11.68749999999999822, -1.946699141100893149 ) ) ;
#7370 = CARTESIAN_POINT ( 'NONE',  ( -3.249999999999999112, 11.81250000000000178, -4.846194077712558723 ) ) ;
#7371 = CARTESIAN_POINT ( 'NONE',  ( 1.346194077712558279, 10.06250000000000000, -6.750000000000000888 ) ) ;
#7372 = ORIENTED_EDGE ( 'NONE', *, *, #6458, .T. ) ;
#7373 = CARTESIAN_POINT ( 'NONE',  ( -6.992168204849981805, 9.999999999999998224, -113.2636094675811762 ) ) ;
#7374 = CARTESIAN_POINT ( 'NONE',  ( 1.346194077712558057, 7.562500000000000000, -6.750000000000000000 ) ) ;
#7375 = CARTESIAN_POINT ( 'NONE',  ( -8.969994997769484613, 1.369616766891445847, -104.6043171117432706 ) ) ;
#7376 = CARTESIAN_POINT ( 'NONE',  ( 13.08366191415227853, 3.715076940595480881, -166.1349492621538957 ) ) ;
#7377 = CARTESIAN_POINT ( 'NONE',  ( 51.19063959271458231, 1.750000000000000000, 70.12932606827693860 ) ) ;
#7378 = COORDINATED_UNIVERSAL_TIME_OFFSET ( 0, 0, .AHEAD. ) ;
#7379 = FACE_BOUND ( 'NONE', #9443, .T. ) ;
#7380 = ORIENTED_EDGE ( 'NONE', *, *, #3195, .F. ) ;
#7381 = CARTESIAN_POINT ( 'NONE',  ( -2.298097038856278918, 2.375000000000000000, -5.798097038856277585 ) ) ;
#7382 = CARTESIAN_POINT ( 'NONE',  ( -2.651650429449553314, 14.37500000000000000, -6.151650429449552426 ) ) ;
#7383 = DIRECTION ( 'NONE',  ( 0.000000000000000000, 1.000000000000000000, 0.000000000000000000 ) ) ;
#7384 = CARTESIAN_POINT ( 'NONE',  ( -4.592425496802573972E-16, 15.00000000000000178, -7.250000000000000000 ) ) ;
#7385 = EDGE_CURVE ( 'NONE', #6553, #2743, #10431, .T. ) ;
#7386 = CARTESIAN_POINT ( 'NONE',  ( -63.45039389062857538, 11.65026692810642750, -203.0695002964987452 ) ) ;
#7387 = CARTESIAN_POINT ( 'NONE',  ( -3.486117781607304345, 9.999999999999998224, -110.4977313129625145 ) ) ;
#7388 = CARTESIAN_POINT ( 'NONE',  ( -3.249999999999999112, 2.812500000000000444, -4.846194077712558723 ) ) ;
#7389 = DIRECTION ( 'NONE',  ( 0.9997619372588932851, -0.000000000000000000, 0.02181900108494707474 ) ) ;
#7390 = APPROVAL_ROLE ( '' ) ;
#7391 = LOCAL_TIME ( 12, 28, 20.00000000000000000, #11788 ) ;
#7392 = CARTESIAN_POINT ( 'NONE',  ( -66.38120458380359423, 14.83440734456928567, -190.9480611771427618 ) ) ;
#7393 = LINE ( 'NONE', #142, #7407 ) ;
#7394 = ORIENTED_EDGE ( 'NONE', *, *, #2891, .F. ) ;
#7395 = CARTESIAN_POINT ( 'NONE',  ( 4.513688785873243958, -0.0008058231150413114373, -1.375597706563020051 ) ) ;
#7396 = CARTESIAN_POINT ( 'NONE',  ( -3.980102097228897245E-16, 6.500000000000000888, -6.749999999999999112 ) ) ;
#7397 = CARTESIAN_POINT ( 'NONE',  ( -8.310659720356554203, 0.7968074792153430064, -105.1373346920393885 ) ) ;
#7398 = CARTESIAN_POINT ( 'NONE',  ( 3.249999999999998668, 13.68750000000000000, -4.846194077712560500 ) ) ;
#7399 = CARTESIAN_POINT ( 'NONE',  ( 2.298097038856278029, 11.12500000000000000, -5.798097038856279362 ) ) ;
#7400 = DIRECTION ( 'NONE',  ( -0.000000000000000000, 0.000000000000000000, 1.000000000000000000 ) ) ;
#7401 = DIRECTION ( 'NONE',  ( 0.000000000000000000, 0.000000000000000000, 1.000000000000000000 ) ) ;
#7402 = CC_DESIGN_SECURITY_CLASSIFICATION ( #8149, ( #15320 ) ) ;
#7403 = CARTESIAN_POINT ( 'NONE',  ( 9.908994292421551719, 14.68779660164460488, -106.4646849496190697 ) ) ;
#7404 = CARTESIAN_POINT ( 'NONE',  ( 3.249999999999999112, 3.812500000000000000, -2.153805922287439945 ) ) ;
#7405 = CARTESIAN_POINT ( 'NONE',  ( -2.651650429449552870, 0.6249999999999998890, -0.8483495705504467965 ) ) ;
#7406 = CIRCLE ( 'NONE', #11840, 1.750000000000001554 ) ;
#7407 = VECTOR ( 'NONE', #1380, 1000.000000000000000 ) ;
#7408 = CARTESIAN_POINT ( 'NONE',  ( 3.749999999999999112, 3.687500000000000444, -5.053300858899108405 ) ) ;
#7409 = EDGE_CURVE ( 'NONE', #14191, #5598, #6976, .T. ) ;
#7410 = CARTESIAN_POINT ( 'NONE',  ( 0.1382019290192771088, 2.747583163733381184, 1.565415805761777301 ) ) ;
#7411 = CARTESIAN_POINT ( 'NONE',  ( 1.553300858899109516, 7.437500000000000000, 0.2499999999999993616 ) ) ;
#7412 = CARTESIAN_POINT ( 'NONE',  ( 4.571546931304953709, 14.29157444506172681, 2.042986306426028076 ) ) ;
#7413 = DIRECTION ( 'NONE',  ( 0.000000000000000000, 1.000000000000000000, 0.000000000000000000 ) ) ;
#7414 = ADVANCED_BREP_SHAPE_REPRESENTATION ( '', ( #12143, #9419 ), #1768 ) ;
#7415 = CARTESIAN_POINT ( 'NONE',  ( 4.492499072540838689, 5.000000000000000000, -2.611025101989581820 ) ) ;
#7416 = AXIS2_PLACEMENT_3D ( 'NONE', #1849, #2859, #10109 ) ;
#7417 = CARTESIAN_POINT ( 'NONE',  ( -66.44604053271804389, 5.000000000000000000, -157.9117883361228394 ) ) ;
#7418 = CARTESIAN_POINT ( 'NONE',  ( 8.895558325401111688, 15.00000000000000000, -125.4560052468458906 ) ) ;
#7419 = CIRCLE ( 'NONE', #6692, 0.2500000000000002220 ) ;
#7420 = CIRCLE ( 'NONE', #8662, 1.000000000000000888 ) ;
#7421 = CARTESIAN_POINT ( 'NONE',  ( 7.013957603348227821, 1.025390859509332619, 1.559562445866058855 ) ) ;
#7422 = VERTEX_POINT ( 'NONE', #5363 ) ;
#7423 = CARTESIAN_POINT ( 'NONE',  ( -3.749999999999999556, 13.75000000000000000, -3.499999999999999112 ) ) ;
#7424 = ORIENTED_EDGE ( 'NONE', *, *, #8346, .F. ) ;
#7425 = CARTESIAN_POINT ( 'NONE',  ( -8.886921396801742645, 15.00000000000000000, -105.5168766094550676 ) ) ;
#7426 = CARTESIAN_POINT ( 'NONE',  ( 10.81715743844561040, 1.218752542932547250E-31, -159.0533339799537487 ) ) ;
#7427 = CARTESIAN_POINT ( 'NONE',  ( 3.749999999999998668, 9.687500000000000000, -5.053300858899107517 ) ) ;
#7428 = CARTESIAN_POINT ( 'NONE',  ( 1.553300858899105963, 8.062500000000001776, -7.249999999999999112 ) ) ;
#7429 = CC_DESIGN_PERSON_AND_ORGANIZATION_ASSIGNMENT ( #11249, #5376, ( #7881 ) ) ;
#7430 = CARTESIAN_POINT ( 'NONE',  ( 3.136841903360915396, 9.999999999999998224, -104.4936450199714955 ) ) ;
#7431 = EDGE_LOOP ( 'NONE', ( #13199, #12501, #9945, #4467 ) ) ;
#7432 = CARTESIAN_POINT ( 'NONE',  ( 3.249999999999999556, 3.250000000000000000, -3.500000000000000000 ) ) ;
#7433 = AXIS2_PLACEMENT_3D ( 'NONE', #9412, #7149, #14137 ) ;
#7434 = EDGE_CURVE ( 'NONE', #1605, #5038, #8290, .T. ) ;
#7435 = CARTESIAN_POINT ( 'NONE',  ( 3.749999999999998668, 10.68750000000000000, -5.053300858899107517 ) ) ;
#7436 = CARTESIAN_POINT ( 'NONE',  ( -64.76906036157818392, 9.999999999999998224, -167.3305518093513058 ) ) ;
#7437 = ADVANCED_FACE ( 'NONE', ( #9523 ), #15116, .F. ) ;
#7438 = EDGE_CURVE ( 'NONE', #9933, #13240, #15192, .T. ) ;
#7439 = CARTESIAN_POINT ( 'NONE',  ( 0.2499999999999999445, 5.000000000000000000, -1.499999999999999778 ) ) ;
#7440 = MANIFOLD_SOLID_BREP ( 'Cortar-Extruir1', #2392 ) ;
#7441 = CARTESIAN_POINT ( 'NONE',  ( -2.298097038856278473, 7.125000000000000000, -1.201902961143720416 ) ) ;
#7442 = CARTESIAN_POINT ( 'NONE',  ( -7.159798565106106238, 14.99999999999025491, -124.1957246867857805 ) ) ;
#7443 = COORDINATED_UNIVERSAL_TIME_OFFSET ( 0, 0, .AHEAD. ) ;
#7444 = CARTESIAN_POINT ( 'NONE',  ( -2.035316908484686937, 5.000000000000002665, -133.6663417172228492 ) ) ;
#7445 = CARTESIAN_POINT ( 'NONE',  ( 8.518838221474071659, 5.000000000000000888, -111.8377054444269589 ) ) ;
#7446 = ORIENTED_EDGE ( 'NONE', *, *, #1290, .F. ) ;
#7447 = CARTESIAN_POINT ( 'NONE',  ( 0.3766621274091715987, 0.5000000000000000000, 0.1491815183709511716 ) ) ;
#7448 = DIRECTION ( 'NONE',  ( 0.9997619372588931741, 0.000000000000000000, 0.02181900108494707474 ) ) ;
#7449 = AXIS2_PLACEMENT_3D ( 'NONE', #9001, #2840, #8700 ) ;
#7450 = VERTEX_POINT ( 'NONE', #14093 ) ;
#7451 = VERTEX_POINT ( 'NONE', #11756 ) ;
#7452 = CARTESIAN_POINT ( 'NONE',  ( -1.376260179405571993, 5.000000000000000000, -106.6458321843530541 ) ) ;
#7453 = CARTESIAN_POINT ( 'NONE',  ( 1.553300858899109071, 12.43750000000000000, 0.2499999999999989175 ) ) ;
#7454 = CARTESIAN_POINT ( 'NONE',  ( 2.298097038856278029, 12.12500000000000000, -5.798097038856279362 ) ) ;
#7455 = CARTESIAN_POINT ( 'NONE',  ( -2.298097038856279362, 9.875000000000000000, -5.798097038856278473 ) ) ;
#7456 = ORIENTED_EDGE ( 'NONE', *, *, #1678, .T. ) ;
#7457 = CARTESIAN_POINT ( 'NONE',  ( 11.32016196459912649, 15.00000000000000000, -106.4092894470390291 ) ) ;
#7458 = CARTESIAN_POINT ( 'NONE',  ( 3.249999999999998668, 6.687500000000000888, -4.846194077712560500 ) ) ;
#7459 = B_SPLINE_CURVE_WITH_KNOTS ( 'NONE', 3,
 ( #322, #14943, #12756, #13767, #4185, #706, #13923, #11357, #9044, #2015, #12448, #1936, #10277, #14868, #3162, #633 ),
 .UNSPECIFIED., .F., .F.,
 ( 4, 2, 2, 2, 2, 2, 2, 4 ),
 ( -1.886160231747189032E-05, 0.0008577525216627750800, 0.001734366645643021891, 0.003487594893603512044, 0.004364209017583777286, 0.005240823141564042963, 0.006117437265544308639, 0.006994051389524575182 ),
 .UNSPECIFIED. ) ;
#7460 = LOCAL_TIME ( 12, 28, 20.00000000000000000, #9415 ) ;
#7461 = CARTESIAN_POINT ( 'NONE',  ( 10.90808873753844033, 14.95946075517707108, -125.5795451959731963 ) ) ;
#7462 = CARTESIAN_POINT ( 'NONE',  ( -46.92959355634174301, 10.00000000000000355, -161.8336071854139959 ) ) ;
#7463 = CARTESIAN_POINT ( 'NONE',  ( 0.000000000000000000, 5.000000000000000000, 0.000000000000000000 ) ) ;
#7464 = COORDINATED_UNIVERSAL_TIME_OFFSET ( 0, 0, .AHEAD. ) ;
#7465 = CARTESIAN_POINT ( 'NONE',  ( -25.17801280822136789, 0.9699280507716093735, -205.4590613150332956 ) ) ;
#7466 = ORIENTED_EDGE ( 'NONE', *, *, #1683, .F. ) ;
#7467 = CARTESIAN_POINT ( 'NONE',  ( 0.000000000000000000, 1.000000000000000000, -0.2500000000000002220 ) ) ;
#7468 = CARTESIAN_POINT ( 'NONE',  ( 1.553300858899108849, 11.93750000000000000, 0.2499999999999993616 ) ) ;
#7469 = ORIENTED_EDGE ( 'NONE', *, *, #6584, .T. ) ;
#7470 = CARTESIAN_POINT ( 'NONE',  ( -10.29275726619092524, 1.020558061026469066, -34.56909192082969184 ) ) ;
#7471 = CARTESIAN_POINT ( 'NONE',  ( -3.749999999999999556, 2.187500000000000444, -1.946699141100892927 ) ) ;
#7472 = CIRCLE ( 'NONE', #5986, 1.771449424009391427 ) ;
#7473 = CARTESIAN_POINT ( 'NONE',  ( -65.57061560049943694, 15.27140727398749220, -203.4644505317938865 ) ) ;
#7474 = CARTESIAN_POINT ( 'NONE',  ( 109.7555300068681419, 1.750000000000000000, 36.44134644672088541 ) ) ;
#7475 = CARTESIAN_POINT ( 'NONE',  ( 11.04730217058844843, 4.659658575842277273, -107.1178495013205350 ) ) ;
#7476 = PERSON_AND_ORGANIZATION ( #3176, #3020 ) ;
#7477 = CARTESIAN_POINT ( 'NONE',  ( -67.58462422314151752, 10.27684056475513685, -204.5041005603981716 ) ) ;
#7478 = FACE_BOUND ( 'NONE', #9679, .T. ) ;
#7479 = APPLICATION_CONTEXT ( 'configuration controlled 3d designs of mechanical parts and assemblies' ) ;
#7480 = VERTEX_POINT ( 'NONE', #96 ) ;
#7481 = CARTESIAN_POINT ( 'NONE',  ( 5.193879428909422558, 0.1412401001306463344, -0.6353294446044706056 ) ) ;
#7482 = CARTESIAN_POINT ( 'NONE',  ( 3.249999999999999112, 7.812500000000000000, -2.153805922287439945 ) ) ;
#7483 = CARTESIAN_POINT ( 'NONE',  ( -8.886921396801763962, 2.500000000000000444, -105.5168766094550676 ) ) ;
#7484 = CARTESIAN_POINT ( 'NONE',  ( -3.249999999999999556, 12.31250000000000000, -4.846194077712557835 ) ) ;
#7485 = CARTESIAN_POINT ( 'NONE',  ( -2.298097038856279362, 10.87499999999999822, -5.798097038856278473 ) ) ;
#7486 = CARTESIAN_POINT ( 'NONE',  ( -0.3803025174127561692, 10.00000000000000000, -103.2080563861792086 ) ) ;
#7487 = CARTESIAN_POINT ( 'NONE',  ( 7.427446726622309647, 5.321094445766562764, -26.41501464507892294 ) ) ;
#7488 = CARTESIAN_POINT ( 'NONE',  ( -10.46704385831657902, 2.500000000000000000, -128.9524512386204549 ) ) ;
#7489 = CARTESIAN_POINT ( 'NONE',  ( -3.249999999999999556, 5.312500000000001776, -4.846194077712557835 ) ) ;
#7490 = CARTESIAN_POINT ( 'NONE',  ( 1.553300858899109071, 4.437499999999999112, 0.2499999999999989175 ) ) ;
#7491 = CARTESIAN_POINT ( 'NONE',  ( 3.749999999999999556, 7.812500000000000000, -1.946699141100892261 ) ) ;
#7492 = CARTESIAN_POINT ( 'NONE',  ( -3.940180586764666870, 10.47454284640667055, -44.50268400149392534 ) ) ;
#7493 = CARTESIAN_POINT ( 'NONE',  ( -3.749999999999999556, 4.750000000000000888, -3.499999999999999112 ) ) ;
#7494 = VECTOR ( 'NONE', #8321, 1000.000000000000000 ) ;
#7495 = CARTESIAN_POINT ( 'NONE',  ( 4.290161713843189339, 13.86208356708933920, 2.954600283075418332 ) ) ;
#7496 = AXIS2_PLACEMENT_3D ( 'NONE', #1074, #5556, #10503 ) ;
#7497 = CARTESIAN_POINT ( 'NONE',  ( 12.23938344417887514, 1.900076854767284829, -165.8029585129606573 ) ) ;
#7498 = CARTESIAN_POINT ( 'NONE',  ( 10.79862538543327410, 3.357576456925632780, -106.9941695556743184 ) ) ;
#7499 = CARTESIAN_POINT ( 'NONE',  ( -11.63193767996857275, 3.999999999999993783, -150.0779743115209897 ) ) ;
#7500 = CARTESIAN_POINT ( 'NONE',  ( 0.000000000000000000, 0.000000000000000000, 0.000000000000000000 ) ) ;
#7501 = CARTESIAN_POINT ( 'NONE',  ( -25.79454819560323031, 8.673617379884037444E-16, -193.5088923898361486 ) ) ;
#7502 = ORIENTED_EDGE ( 'NONE', *, *, #1400, .F. ) ;
#7503 = EDGE_CURVE ( 'NONE', #14756, #14271, #14244, .T. ) ;
#7504 = CARTESIAN_POINT ( 'NONE',  ( 3.249999999999999556, 0.2500000000000001110, -3.500000000000000000 ) ) ;
#7505 = ORIENTED_EDGE ( 'NONE', *, *, #6671, .F. ) ;
#7506 = DIRECTION ( 'NONE',  ( 0.000000000000000000, 0.000000000000000000, 1.000000000000000000 ) ) ;
#7507 = CARTESIAN_POINT ( 'NONE',  ( -15.21741835282884381, 3.999999999999802380, -192.8143658740737010 ) ) ;
#7508 = CARTESIAN_POINT ( 'NONE',  ( 2.651650429449552870, 9.625000000000000000, -6.151650429449554203 ) ) ;
#7509 = AXIS2_PLACEMENT_3D ( 'NONE', #10691, #7202, #11920 ) ;
#7510 = CARTESIAN_POINT ( 'NONE',  ( 3.749999999999999556, 8.250000000000000000, -3.500000000000000444 ) ) ;
#7511 = FACE_OUTER_BOUND ( 'NONE', #15120, .T. ) ;
#7512 = ORIENTED_EDGE ( 'NONE', *, *, #4344, .T. ) ;
#7513 = CARTESIAN_POINT ( 'NONE',  ( 2.298097038856279362, 6.374999999999999112, -1.201902961143720860 ) ) ;
#7514 = CARTESIAN_POINT ( 'NONE',  ( -2.651650429449552870, 11.12500000000000000, -0.8483495705504462414 ) ) ;
#7515 = CARTESIAN_POINT ( 'NONE',  ( -61.92089974418476572, 15.00000000000000000, -174.1061791381038404 ) ) ;
#7516 = LINE ( 'NONE', #3037, #2736 ) ;
#7517 = DIRECTION ( 'NONE',  ( 0.000000000000000000, 0.000000000000000000, 1.000000000000000000 ) ) ;
#7518 = CARTESIAN_POINT ( 'NONE',  ( 1.346194077712560944, 9.937499999999998224, -0.2500000000000010547 ) ) ;
#7519 = AXIS2_PLACEMENT_3D ( 'NONE', #4633, #1000, #14066 ) ;
#7520 = CARTESIAN_POINT ( 'NONE',  ( -3.538505488862558224, 15.00000000000000711, -119.6277774347352079 ) ) ;
#7521 = CARTESIAN_POINT ( 'NONE',  ( -8.651617673336016168, 2.768730321972320486E-12, -120.1343837247038380 ) ) ;
#7522 = CARTESIAN_POINT ( 'NONE',  ( 11.18419171849476790, 1.127570259384924454E-14, -106.9754176129513752 ) ) ;
#7523 = ORIENTED_EDGE ( 'NONE', *, *, #13014, .T. ) ;
#7524 = CARTESIAN_POINT ( 'NONE',  ( 4.999999999999999112, 0.000000000000000000, -100.6237003951525679 ) ) ;
#7525 = DIRECTION ( 'NONE',  ( -0.08794243244722420305, 1.868163743359636407E-15, -0.9961255586397055328 ) ) ;
#7526 = VERTEX_POINT ( 'NONE', #10530 ) ;
#7527 = EDGE_CURVE ( 'NONE', #14187, #13643, #1251, .T. ) ;
#7528 = CARTESIAN_POINT ( 'NONE',  ( -65.53364736412717662, 15.00000000000000000, -203.4171941195418754 ) ) ;
#7529 = CARTESIAN_POINT ( 'NONE',  ( 21.60584812306049329, 0.02716718192045389224, -138.8895968602480195 ) ) ;
#7530 = CARTESIAN_POINT ( 'NONE',  ( -4.592425496802573972E-16, 14.00000000000000000, -7.250000000000000000 ) ) ;
#7531 = CARTESIAN_POINT ( 'NONE',  ( 3.249999999999999556, 13.25000000000000178, -3.500000000000000000 ) ) ;
#7532 = EDGE_CURVE ( 'NONE', #559, #1425, #4809, .T. ) ;
#7533 = CARTESIAN_POINT ( 'NONE',  ( -1.346194077712558945, 11.56250000000000178, -0.2500000000000002220 ) ) ;
#7534 = ORIENTED_EDGE ( 'NONE', *, *, #14289, .T. ) ;
#7535 = CARTESIAN_POINT ( 'NONE',  ( -3.648797883638980277, -2.490287375297125294, -1.000000000000000888 ) ) ;
#7536 = CARTESIAN_POINT ( 'NONE',  ( 0.000000000000000000, 9.000000000000001776, -0.2500000000000002220 ) ) ;
#7537 = CARTESIAN_POINT ( 'NONE',  ( -4.090890948359604984, 15.00000000000000000, -103.1929727064838147 ) ) ;
#7538 = CARTESIAN_POINT ( 'NONE',  ( -2.256557393256121369, 5.321094445766560987, -25.56006732368493317 ) ) ;
#7539 = CARTESIAN_POINT ( 'NONE',  ( -4.234402844927157794, 15.00000000000000000, -117.4888040839639558 ) ) ;
#7540 = SECURITY_CLASSIFICATION_LEVEL ( 'unclassified' ) ;
#7541 = DIRECTION ( 'NONE',  ( 0.9939692226109180240, -0.000000000000000000, -0.1096594022519158940 ) ) ;
#7542 = ORIENTED_EDGE ( 'NONE', *, *, #7434, .T. ) ;
#7543 = MANIFOLD_SOLID_BREP ( 'Saliente-Extruir1', #3893 ) ;
#7544 = CARTESIAN_POINT ( 'NONE',  ( 1.346194077712558057, 1.562500000000000000, -6.750000000000000000 ) ) ;
#7545 = CARTESIAN_POINT ( 'NONE',  ( -3.750000000000000000, -0.3124999999999999445, -1.946699141100893149 ) ) ;
#7546 = ADVANCED_FACE ( 'NONE', ( #15263 ), #11487, .T. ) ;
#7547 = ORIENTED_EDGE ( 'NONE', *, *, #8268, .T. ) ;
#7548 = DIRECTION ( 'NONE',  ( 0.000000000000000000, 0.000000000000000000, -1.000000000000000000 ) ) ;
#7550 = CARTESIAN_POINT ( 'NONE',  ( 3.750000000000000000, 0.7500000000000000000, -3.500000000000000444 ) ) ;
#7549 =( BOUNDED_SURFACE ( )  B_SPLINE_SURFACE ( 3, 1, ( 
 ( #1362, #8462 ),
 ( #6380, #13196 ),
 ( #2601, #9861 ),
 ( #9709, #7300 ) ),
 .UNSPECIFIED., .F., .F., .T. ) 
 B_SPLINE_SURFACE_WITH_KNOTS ( ( 4, 4 ),
 ( 2, 2 ),
 ( 0.000000000000000000, 1.000000000000000000 ),
 ( 0.000000000000000000, 1.000000000000000000 ),
 .UNSPECIFIED. ) 
 GEOMETRIC_REPRESENTATION_ITEM ( )  RATIONAL_B_SPLINE_SURFACE ( (
 ( 1.000000000000000000, 1.000000000000000000),
 ( 0.6867676532959785529, 0.6867676532959785529),
 ( 0.6867676532959785529, 0.6867676532959785529),
 ( 1.000000000000000000, 1.000000000000000000) ) ) 
 REPRESENTATION_ITEM ( '' )  SURFACE ( )  );
#7551 = CARTESIAN_POINT ( 'NONE',  ( 7.375268436326912536, 3.304579630018633196, -22.32553049743219376 ) ) ;
#7552 = CARTESIAN_POINT ( 'NONE',  ( 3.111877744625329623, 1.934442845508696607, 4.175147216457742338 ) ) ;
#7553 = CARTESIAN_POINT ( 'NONE',  ( 2.651650429449552870, 0.6250000000000000000, -6.151650429449554203 ) ) ;
#7554 = COORDINATED_UNIVERSAL_TIME_OFFSET ( 0, 0, .AHEAD. ) ;
#7555 = CARTESIAN_POINT ( 'NONE',  ( -67.58984843273714205, 10.68251503306532690, -204.4107792426363801 ) ) ;
#7556 = DIRECTION ( 'NONE',  ( -0.9997619372588932851, 0.000000000000000000, -0.02181900108494707474 ) ) ;
#7557 = ORIENTED_EDGE ( 'NONE', *, *, #13517, .F. ) ;
#7558 = CARTESIAN_POINT ( 'NONE',  ( 3.249999999999999556, 8.750000000000000000, -3.500000000000000000 ) ) ;
#7559 = CARTESIAN_POINT ( 'NONE',  ( -0.9087754948914270603, 2.490287375297123962, -36.05536862169275025 ) ) ;
#7560 = CARTESIAN_POINT ( 'NONE',  ( -3.249999999999999556, 14.31250000000000000, -4.846194077712557835 ) ) ;
#7561 = CARTESIAN_POINT ( 'NONE',  ( 2.298097038856278029, 12.12500000000000000, -5.798097038856279362 ) ) ;
#7562 = CARTESIAN_POINT ( 'NONE',  ( -1.653263949012560463, 10.00000000000000000, -106.3284344075506738 ) ) ;
#7563 = CARTESIAN_POINT ( 'NONE',  ( 11.32911568800036584, 12.49999999999999822, -106.8195553349433169 ) ) ;
#7564 = CARTESIAN_POINT ( 'NONE',  ( 2.298097038856278473, 6.625000000000000000, -5.798097038856279362 ) ) ;
#7565 = CARTESIAN_POINT ( 'NONE',  ( 0.000000000000000000, 3.500000000000000000, 0.2499999999999998057 ) ) ;
#7566 = CARTESIAN_POINT ( 'NONE',  ( -2.651650429449553314, 10.37500000000000000, -6.151650429449552426 ) ) ;
#7567 = DIRECTION ( 'NONE',  ( 0.000000000000000000, 1.000000000000000000, 0.000000000000000000 ) ) ;
#7568 = CARTESIAN_POINT ( 'NONE',  ( 0.2553636793526916082, 4.345756845072476615, 2.892509118448076677 ) ) ;
#7569 = CARTESIAN_POINT ( 'NONE',  ( 1.553300858899105963, 10.06250000000000000, -7.250000000000000888 ) ) ;
#7570 = CARTESIAN_POINT ( 'NONE',  ( 4.516489297216762289, -0.0008961263506977127508, -1.658221315985885846 ) ) ;
#7571 = CARTESIAN_POINT ( 'NONE',  ( 13.02619977026641074, 3.477781664713968990, -166.0928117978999126 ) ) ;
#7572 = CARTESIAN_POINT ( 'NONE',  ( 1.635615696801046015, 1.750000000000000000, -0.6802899045268993028 ) ) ;
#7573 = CARTESIAN_POINT ( 'NONE',  ( -21.49024324108596318, 3.999999999999993783, -163.1063489299302773 ) ) ;
#7574 = CARTESIAN_POINT ( 'NONE',  ( 5.536303798911983876, 0.008884980407317709730, -141.3787188740540444 ) ) ;
#7575 = DESIGN_CONTEXT ( 'detailed design', #15111, 'design' ) ;
#7576 = CARTESIAN_POINT ( 'NONE',  ( -6.930553666837859339, 8.673617379884034486E-16, -152.1805032840957779 ) ) ;
#7577 = CARTESIAN_POINT ( 'NONE',  ( -3.249999999999999556, 0.7500000000000001110, -3.500000000000000000 ) ) ;
#7578 = ORIENTED_EDGE ( 'NONE', *, *, #10885, .T. ) ;
#7579 = CYLINDRICAL_SURFACE ( 'NONE', #7243, 2.500000000000000444 ) ;
#7580 = CARTESIAN_POINT ( 'NONE',  ( 8.780952025204904032, 0.6450331482581128650, -105.6724537816508729 ) ) ;
#7581 = CARTESIAN_POINT ( 'NONE',  ( 1.553300858899105963, 7.562500000000000000, -7.250000000000000888 ) ) ;
#7582 = CARTESIAN_POINT ( 'NONE',  ( 2.651650429449552870, 10.12500000000000000, -6.151650429449553314 ) ) ;
#7583 = DIRECTION ( 'NONE',  ( -0.000000000000000000, 1.000000000000000000, -0.000000000000000000 ) ) ;
#7584 = CARTESIAN_POINT ( 'NONE',  ( 1.346194077712558279, 9.062500000000003553, -6.750000000000000888 ) ) ;
#7585 = B_SPLINE_CURVE_WITH_KNOTS ( 'NONE', 3,
 ( #3084, #11347, #2003, #7798, #5481, #10199, #5257, #14707, #4107, #2937 ),
 .UNSPECIFIED., .F., .F.,
 ( 4, 2, 2, 2, 4 ),
 ( 0.000000000000000000, 0.0002702708960404937824, 0.0005405417920809875649, 0.0008108126881214814015, 0.001081083584161975130 ),
 .UNSPECIFIED. ) ;
#7586 = CARTESIAN_POINT ( 'NONE',  ( -1.553300858899107295, 14.43750000000000000, -7.250000000000000000 ) ) ;
#7587 = DIRECTION ( 'NONE',  ( 0.000000000000000000, 0.000000000000000000, -1.000000000000000000 ) ) ;
#7588 = CARTESIAN_POINT ( 'NONE',  ( -8.090126491280004828, 5.000000000000000000, -136.8653377734624996 ) ) ;
#7589 = ADVANCED_FACE ( 'NONE', ( #11065 ), #13056, .F. ) ;
#7590 =( NAMED_UNIT ( * ) PLANE_ANGLE_UNIT ( ) SI_UNIT ( $, .RADIAN. ) );
#7591 = CARTESIAN_POINT ( 'NONE',  ( -3.249999999999999556, 13.31250000000000000, -4.846194077712557835 ) ) ;
#7592 = CARTESIAN_POINT ( 'NONE',  ( 5.228075279701640099, 1.000000000000000000, -163.7939279834373849 ) ) ;
#7593 = LINE ( 'NONE', #6049, #2083 ) ;
#7594 = CARTESIAN_POINT ( 'NONE',  ( 8.592224267391641135, 8.673617379884035472E-16, -111.5170830772493957 ) ) ;
#7595 = DIRECTION ( 'NONE',  ( -0.000000000000000000, -1.000000000000000000, -0.000000000000000000 ) ) ;
#7596 = CARTESIAN_POINT ( 'NONE',  ( 0.000000000000000000, 15.00000000000000000, 0.000000000000000000 ) ) ;
#7597 = ORIENTED_EDGE ( 'NONE', *, *, #1584, .T. ) ;
#7598 = CARTESIAN_POINT ( 'NONE',  ( 1.052436484934202499, -2.075239479414269894, -1.000000000000000888 ) ) ;
#7599 = CARTESIAN_POINT ( 'NONE',  ( -0.3766621274091715987, 0.2613176957160640579, -6.863050255469941519 ) ) ;
#7600 = CARTESIAN_POINT ( 'NONE',  ( -3.750000000000000000, 13.68750000000000178, -1.946699141100893149 ) ) ;
#7601 = CARTESIAN_POINT ( 'NONE',  ( -2.298097038856279362, 11.87500000000000000, -5.798097038856278473 ) ) ;
#7602 = EDGE_CURVE ( 'NONE', #7276, #8407, #4076, .T. ) ;
#7603 = CARTESIAN_POINT ( 'NONE',  ( 1.346194077712560944, 1.937500000000000000, -0.2500000000000010547 ) ) ;
#7604 = ORIENTED_EDGE ( 'NONE', *, *, #2525, .F. ) ;
#7605 = B_SPLINE_CURVE_WITH_KNOTS ( 'NONE', 3,
 ( #13234, #11819, #2636, #14237, #3638, #7338, #8340, #12051, #10746, #6182, #7176, #10901, #319, #1323 ),
 .UNSPECIFIED., .F., .F.,
 ( 4, 2, 2, 2, 2, 2, 4 ),
 ( -1.076617132515563425E-05, 0.0009993995386319133676, 0.002009565248588982347, 0.002514648103567523017, 0.003019730958546064121, 0.003524813813524604791, 0.004029896668503145027 ),
 .UNSPECIFIED. ) ;
#7606 = CARTESIAN_POINT ( 'NONE',  ( 3.249999999999998668, 9.687500000000000000, -4.846194077712560500 ) ) ;
#7607 = CARTESIAN_POINT ( 'NONE',  ( 4.675143156396779354, 2.724689664222763125E-15, -31.08615533255463603 ) ) ;
#7608 = CARTESIAN_POINT ( 'NONE',  ( -8.886921396801742645, 2.500000000000000444, -105.5168766094550676 ) ) ;
#7609 = CARTESIAN_POINT ( 'NONE',  ( 5.163630139845929889, 1.524494085803895782, 3.626316403462681137 ) ) ;
#7610 = CARTESIAN_POINT ( 'NONE',  ( -6.822452048367190436, 14.42304080573416236, -117.0063474466252558 ) ) ;
#7611 = EDGE_CURVE ( 'NONE', #5990, #3511, #14669, .T. ) ;
#7612 = PERSON_AND_ORGANIZATION ( #3176, #3020 ) ;
#7613 = CARTESIAN_POINT ( 'NONE',  ( -25.31190114102989597, 0.4153624176314577032, -203.6532684513659888 ) ) ;
#7614 = ORIENTED_EDGE ( 'NONE', *, *, #6843, .T. ) ;
#7615 = CARTESIAN_POINT ( 'NONE',  ( -3.249999999999999112, 13.68750000000000178, -2.153805922287440833 ) ) ;
#7616 = CARTESIAN_POINT ( 'NONE',  ( -1.553300858899106629, -0.4374999999999998890, 0.2500000000000002220 ) ) ;
#7617 = ORIENTED_EDGE ( 'NONE', *, *, #14636, .F. ) ;
#7618 = FACE_OUTER_BOUND ( 'NONE', #1600, .T. ) ;
#7619 = CC_DESIGN_PERSON_AND_ORGANIZATION_ASSIGNMENT ( #6982, #11699, ( #8149 ) ) ;
#7620 = CARTESIAN_POINT ( 'NONE',  ( 2.651650429449552870, 2.625000000000000000, -6.151650429449554203 ) ) ;
#7621 = DIRECTION ( 'NONE',  ( 0.000000000000000000, 0.000000000000000000, -1.000000000000000000 ) ) ;
#7622 = EDGE_CURVE ( 'NONE', #7799, #12868, #8453, .T. ) ;
#7623 = CARTESIAN_POINT ( 'NONE',  ( 0.1865797813170224362, 3.107330460720267418, 2.113392633384786556 ) ) ;
#7624 = CARTESIAN_POINT ( 'NONE',  ( -3.750000000000000000, 2.312500000000000888, -5.053300858899105741 ) ) ;
#7625 = ADVANCED_FACE ( 'NONE', ( #11219 ), #8746, .T. ) ;
#7626 = APPROVAL_DATE_TIME ( #3002, #15090 ) ;
#7627 = EDGE_CURVE ( 'NONE', #6503, #10346, #6730, .T. ) ;
#7628 = FACE_OUTER_BOUND ( 'NONE', #13354, .T. ) ;
#7629 = DIRECTION ( 'NONE',  ( -0.000000000000000000, -1.000000000000000000, -0.000000000000000000 ) ) ;
#7630 = ORIENTED_EDGE ( 'NONE', *, *, #12922, .F. ) ;
#7631 = CARTESIAN_POINT ( 'NONE',  ( -3.249999999999999556, 10.18750000000000000, -2.153805922287440833 ) ) ;
#7632 = CARTESIAN_POINT ( 'NONE',  ( -69.52150835262156647, 10.00000000000000178, -199.0124118306254957 ) ) ;
#7633 = CARTESIAN_POINT ( 'NONE',  ( -2.298097038856278029, 4.624999999999999112, -1.201902961143720638 ) ) ;
#7634 = CARTESIAN_POINT ( 'NONE',  ( -2.298097038856278029, 12.62500000000000000, -1.201902961143720638 ) ) ;
#7635 = CARTESIAN_POINT ( 'NONE',  ( -5.285700560996287045, 15.00000000000000000, -102.0031443936493787 ) ) ;
#7636 = SHAPE_REPRESENTATION ( 'PruningShears_Predeterminado', ( #9419 ), #3238 ) ;
#7637 = CARTESIAN_POINT ( 'NONE',  ( 10.47455747790057679, 14.18553633661278113, -106.7841271890158765 ) ) ;
#7638 = CARTESIAN_POINT ( 'NONE',  ( 1.346194077712558057, 3.562500000000000444, -6.750000000000000000 ) ) ;
#7639 = CARTESIAN_POINT ( 'NONE',  ( -2.651650429449552870, 4.624999999999999112, -0.8483495705504467965 ) ) ;
#7640 = CARTESIAN_POINT ( 'NONE',  ( -3.750000000000000000, 9.312500000000000000, -5.053300858899105741 ) ) ;
#7641 = APPROVAL_PERSON_ORGANIZATION ( #5988, #12728, #201 ) ;
#7642 = DIRECTION ( 'NONE',  ( 0.000000000000000000, -1.000000000000000000, 0.000000000000000000 ) ) ;
#7643 = DIRECTION ( 'NONE',  ( -0.08794243244722425856, -0.000000000000000000, -0.9961255586397054218 ) ) ;
#7644 = CARTESIAN_POINT ( 'NONE',  ( -3.750000000000000000, 11.81250000000000178, -5.053300858899105741 ) ) ;
#7645 = DIRECTION ( 'NONE',  ( 0.000000000000000000, 0.000000000000000000, 1.000000000000000000 ) ) ;
#7646 = VECTOR ( 'NONE', #13717, 1000.000000000000000 ) ;
#7647 = DIRECTION ( 'NONE',  ( 0.000000000000000000, 0.000000000000000000, 1.000000000000000000 ) ) ;
#7648 = AXIS2_PLACEMENT_3D ( 'NONE', #9110, #15085, #13836 ) ;
#7649 = CARTESIAN_POINT ( 'NONE',  ( 11.01519796548710417, 4.326353643838777074, -107.1017525683475498 ) ) ;
#7650 = CC_DESIGN_PERSON_AND_ORGANIZATION_ASSIGNMENT ( #5851, #1075, ( #8939 ) ) ;
#7651 = CARTESIAN_POINT ( 'NONE',  ( -12.13691226097295228, 8.673617379884034486E-16, -151.8391917678144694 ) ) ;
#7652 = LINE ( 'NONE', #5035, #10145 ) ;
#7653 = CARTESIAN_POINT ( 'NONE',  ( -47.49849438531821733, 9.999999999999998224, -162.3383809241888400 ) ) ;
#7654 = SECURITY_CLASSIFICATION ( '', '', #14260 ) ;
#7655 = CARTESIAN_POINT ( 'NONE',  ( -2.651650429449552870, 12.62500000000000000, -0.8483495705504463524 ) ) ;
#7656 = ORIENTED_EDGE ( 'NONE', *, *, #14056, .F. ) ;
#7657 = DIRECTION ( 'NONE',  ( 0.000000000000000000, 0.000000000000000000, -1.000000000000000000 ) ) ;
#7658 = CARTESIAN_POINT ( 'NONE',  ( -8.167870570054514445, 5.000000000000000888, -136.8278529952039264 ) ) ;
#7659 = CARTESIAN_POINT ( 'NONE',  ( -2.651650429449552870, 8.625000000000000000, -0.8483495705504467965 ) ) ;
#7660 = CIRCLE ( 'NONE', #11, 9.500954284471095690 ) ;
#7661 = CARTESIAN_POINT ( 'NONE',  ( 4.248871783098695509, 6.000000000000000000, -126.1456066832003842 ) ) ;
#7662 = CARTESIAN_POINT ( 'NONE',  ( -2.298097038856278029, 7.625000000000000000, -1.201902961143720638 ) ) ;
#7663 = CARTESIAN_POINT ( 'NONE',  ( -15.73004658022870927, 0.000000000000000000, -131.7446186346720367 ) ) ;
#7664 = CARTESIAN_POINT ( 'NONE',  ( -4.592425496802573972E-16, 12.50000000000000000, -7.249999999999999112 ) ) ;
#7665 = CARTESIAN_POINT ( 'NONE',  ( -69.06832266641278295, 15.00000000000115463, -200.7467498276384106 ) ) ;
#7666 = AXIS2_PLACEMENT_3D ( 'NONE', #2586, #12310, #2894 ) ;
#7667 = DIRECTION ( 'NONE',  ( 0.08794243244723021213, 0.000000000000000000, 0.9961255586397049777 ) ) ;
#7668 = APPROVAL_DATE_TIME ( #1648, #4519 ) ;
#7669 = CARTESIAN_POINT ( 'NONE',  ( 2.298097038856278473, 10.62500000000000000, -5.798097038856279362 ) ) ;
#7670 = VECTOR ( 'NONE', #3016, 999.9999999999998863 ) ;
#7671 = CARTESIAN_POINT ( 'NONE',  ( -5.538855545106806666, 10.00000000000000000, -110.3982026382703765 ) ) ;
#7672 = AXIS2_PLACEMENT_3D ( 'NONE', #13527, #6325, #4167 ) ;
#7673 = CARTESIAN_POINT ( 'NONE',  ( 8.935548306746154523, 15.00000000000000000, 2.855381328098122395 ) ) ;
#7674 = CARTESIAN_POINT ( 'NONE',  ( 5.457768971991409757, 8.673617379884035472E-16, -106.2114798315073614 ) ) ;
#7675 = CARTESIAN_POINT ( 'NONE',  ( 3.158745454532927877, 2.478737181588197558, 4.576782562779927233 ) ) ;
#7676 = DIRECTION ( 'NONE',  ( -1.000000000000000000, -0.000000000000000000, -0.000000000000000000 ) ) ;
#7677 = ORIENTED_EDGE ( 'NONE', *, *, #12902, .F. ) ;
#7678 = ADVANCED_FACE ( 'NONE', ( #8971 ), #10404, .T. ) ;
#7679 = CARTESIAN_POINT ( 'NONE',  ( 9.950255046238396517, 5.943472311793079221, -43.63919336277970018 ) ) ;
#7680 = CARTESIAN_POINT ( 'NONE',  ( 0.2116200952963270543, 15.00000000000000178, -112.6243614187691975 ) ) ;
#7681 = CARTESIAN_POINT ( 'NONE',  ( -2.651650429449552870, 14.87500000000000355, -6.151650429449552426 ) ) ;
#7682 = CARTESIAN_POINT ( 'NONE',  ( 3.249999999999998224, 12.31250000000000178, -2.153805922287439945 ) ) ;
#7683 = CARTESIAN_POINT ( 'NONE',  ( -3.249999999999999556, 12.74999999999999822, -3.500000000000000000 ) ) ;
#7684 = ORIENTED_EDGE ( 'NONE', *, *, #12408, .F. ) ;
#7685 = AXIS2_PLACEMENT_3D ( 'NONE', #7463, #2841, #13435 ) ;
#7686 = CARTESIAN_POINT ( 'NONE',  ( -2.298097038856278918, 10.37500000000000000, -5.798097038856277585 ) ) ;
#7687 = CARTESIAN_POINT ( 'NONE',  ( 9.995755633401696372, 11.56847231179307833, -45.72406218842818504 ) ) ;
#7688 = CARTESIAN_POINT ( 'NONE',  ( -6.167185496248319687, 14.52912145062034455, -104.1275751645885776 ) ) ;
#7689 = FACE_OUTER_BOUND ( 'NONE', #2359, .T. ) ;
#7690 = CARTESIAN_POINT ( 'NONE',  ( -9.192419678266180227, 11.41184093590166349, -115.4428990047099148 ) ) ;
#7691 = PERSON_AND_ORGANIZATION ( #3176, #3020 ) ;
#7692 = CARTESIAN_POINT ( 'NONE',  ( 8.507048280435965282, 12.49999999999999822, -111.8750672985880499 ) ) ;
#7693 = VERTEX_POINT ( 'NONE', #14721 ) ;
#7694 = TOROIDAL_SURFACE ( 'NONE', #10162, 2.000000000000011990, 1.000000000000000000 ) ;
#7695 = CARTESIAN_POINT ( 'NONE',  ( 2.298097038856279362, 4.875000000000000000, -1.201902961143720860 ) ) ;
#7696 = DIRECTION ( 'NONE',  ( -0.02181900108494707474, 0.000000000000000000, 0.9997619372588932851 ) ) ;
#7697 = CARTESIAN_POINT ( 'NONE',  ( 3.750000000000000000, 12.75000000000000178, -3.500000000000000444 ) ) ;
#7698 = ORIENTED_EDGE ( 'NONE', *, *, #2677, .F. ) ;
#7699 = ADVANCED_FACE ( 'NONE', ( #11142 ), #11897, .T. ) ;
#7700 = CARTESIAN_POINT ( 'NONE',  ( -4.887975900231274373, 14.97051500633131305, -117.2415000213202916 ) ) ;
#7701 = APPROVAL_PERSON_ORGANIZATION ( #12273, #10068, #7390 ) ;
#7702 = CARTESIAN_POINT ( 'NONE',  ( -1.553300858899106629, 3.062500000000000000, 0.2500000000000002220 ) ) ;
#7703 = DIRECTION ( 'NONE',  ( -0.05964429961207245307, 0.000000000000000000, -0.9982196940171964572 ) ) ;
#7704 = CARTESIAN_POINT ( 'NONE',  ( 0.2550590916302901690, 4.348754961233985306, 2.889059047683731229 ) ) ;
#7705 = CARTESIAN_POINT ( 'NONE',  ( 3.749999999999999112, 0.6875000000000000000, -5.053300858899108405 ) ) ;
#7706 = COORDINATED_UNIVERSAL_TIME_OFFSET ( 0, 0, .AHEAD. ) ;
#7707 = CARTESIAN_POINT ( 'NONE',  ( 8.432848914831144072, 5.000000000000002665, -115.6062006120311878 ) ) ;
#7708 = DIRECTION ( 'NONE',  ( 0.000000000000000000, 0.000000000000000000, 1.000000000000000000 ) ) ;
#7709 = CC_DESIGN_APPROVAL ( #6528, ( #10666 ) ) ;
#7710 = ORIENTED_EDGE ( 'NONE', *, *, #2236, .F. ) ;
#7711 = CARTESIAN_POINT ( 'NONE',  ( -0.9087754948914270603, -2.075239479414269894, -36.05536862169275025 ) ) ;
#7712 = CARTESIAN_POINT ( 'NONE',  ( -3.249999999999999112, 3.812500000000000000, -4.846194077712558723 ) ) ;
#7713 = ADVANCED_FACE ( 'NONE', ( #2020 ), #5006, .T. ) ;
#7714 = CARTESIAN_POINT ( 'NONE',  ( -1.346194077712559167, 10.93750000000000000, -6.749999999999999112 ) ) ;
#7715 = CARTESIAN_POINT ( 'NONE',  ( -7.575942540376401801, 9.999999999999998224, -106.7905032256467734 ) ) ;
#7716 = VECTOR ( 'NONE', #3496, 1000.000000000000000 ) ;
#7717 = EDGE_CURVE ( 'NONE', #5516, #1192, #3808, .T. ) ;
#7718 = EDGE_CURVE ( 'NONE', #10451, #1120, #10135, .T. ) ;
#7719 = CARTESIAN_POINT ( 'NONE',  ( -2.298097038856278473, 7.125000000000000000, -1.201902961143720416 ) ) ;
#7720 = CARTESIAN_POINT ( 'NONE',  ( 2.651650429449552870, 6.125000000000000000, -6.151650429449553314 ) ) ;
#7721 = CARTESIAN_POINT ( 'NONE',  ( -3.750000000000000000, 9.250000000000000000, -3.499999999999999112 ) ) ;
#7722 = CARTESIAN_POINT ( 'NONE',  ( -9.097645849187591338, 3.303830902112122825, -115.4858344565725616 ) ) ;
#7723 = LINE ( 'NONE', #6641, #3731 ) ;
#7724 = CC_DESIGN_PERSON_AND_ORGANIZATION_ASSIGNMENT ( #13835, #5557, ( #7950 ) ) ;
#7725 = CARTESIAN_POINT ( 'NONE',  ( 3.750000000000000000, 8.312500000000003553, -1.946699141100892705 ) ) ;
#7726 = CARTESIAN_POINT ( 'NONE',  ( 4.837808514977005814, -1.933783910781458629E-11, -31.10787113836400763 ) ) ;
#7727 = DIRECTION ( 'NONE',  ( 0.000000000000000000, 0.000000000000000000, -1.000000000000000000 ) ) ;
#7728 = TOROIDAL_SURFACE ( 'NONE', #11676, 2.000000000000016431, 5.000000000000000000 ) ;
#7729 = DIRECTION ( 'NONE',  ( -0.6876103830954231055, -9.542510991048287223E-16, 0.7260798585963982310 ) ) ;
#7730 = CARTESIAN_POINT ( 'NONE',  ( -25.06351876112395161, 0.000000000000000000, -185.5277672829032838 ) ) ;
#7731 = CARTESIAN_POINT ( 'NONE',  ( 2.298097038856279362, 0.8750000000000000000, -1.201902961143720860 ) ) ;
#7732 = CARTESIAN_POINT ( 'NONE',  ( -36.12930860109405273, 9.999999999999998224, -156.3173234977680011 ) ) ;
#7733 = CARTESIAN_POINT ( 'NONE',  ( -2.298097038856279362, -0.1249999999999999029, -5.798097038856278473 ) ) ;
#7734 = ORIENTED_EDGE ( 'NONE', *, *, #8656, .T. ) ;
#7735 = LINE ( 'NONE', #7425, #1336 ) ;
#7736 = CARTESIAN_POINT ( 'NONE',  ( 11.15078183098557218, 3.671353358600427441, -106.3578943783445823 ) ) ;
#7737 = ADVANCED_FACE ( 'NONE', ( #10131 ), #11290, .F. ) ;
#7738 = DIRECTION ( 'NONE',  ( 0.000000000000000000, 0.000000000000000000, 1.000000000000000000 ) ) ;
#7739 = PRODUCT_RELATED_PRODUCT_CATEGORY ( 'detail', '', ( #4992 ) ) ;
#7740 = CARTESIAN_POINT ( 'NONE',  ( -9.817351912531890434, 4.222959489602541083, -115.7707972434356378 ) ) ;
#7741 = CIRCLE ( 'NONE', #7981, 4.000000000000000000 ) ;
#7742 = CARTESIAN_POINT ( 'NONE',  ( 3.249999999999998224, 7.312500000000000000, -2.153805922287439945 ) ) ;
#7743 = CIRCLE ( 'NONE', #3058, 3.500000000000003109 ) ;
#7744 = LINE ( 'NONE', #14954, #13112 ) ;
#7745 = CARTESIAN_POINT ( 'NONE',  ( 1.553300858899105963, 13.56250000000000000, -7.250000000000000888 ) ) ;
#7746 = LINE ( 'NONE', #5575, #3961 ) ;
#7747 = LINE ( 'NONE', #1572, #2232 ) ;
#7748 = CARTESIAN_POINT ( 'NONE',  ( 2.298097038856278473, 13.62500000000000000, -5.798097038856279362 ) ) ;
#7749 = LINE ( 'NONE', #7592, #4380 ) ;
#7750 = CARTESIAN_POINT ( 'NONE',  ( 4.891108815300913015, 14.90343850142792270, -1.429801464957401347 ) ) ;
#7751 = CARTESIAN_POINT ( 'NONE',  ( 3.249999999999999556, 6.750000000000000000, -3.500000000000000000 ) ) ;
#7752 = CIRCLE ( 'NONE', #6278, 2.326940983401415419 ) ;
#7753 = AXIS2_PLACEMENT_3D ( 'NONE', #1561, #6504, #13700 ) ;
#7754 = CARTESIAN_POINT ( 'NONE',  ( 10.95491677860929869, 11.75663172244964727, -44.24084729402226657 ) ) ;
#7755 = B_SPLINE_CURVE_WITH_KNOTS ( 'NONE', 3,
 ( #13099, #6056, #4830, #4751 ),
 .UNSPECIFIED., .F., .F.,
 ( 4, 4 ),
 ( 0.000000000000000000, 0.0003766621653985018536 ),
 .UNSPECIFIED. ) ;
#7756 = ORIENTED_EDGE ( 'NONE', *, *, #2031, .F. ) ;
#7757 = CARTESIAN_POINT ( 'NONE',  ( 8.976483039626360849, 12.42182331701315867, 0.9797231489651803127 ) ) ;
#7758 = DIRECTION ( 'NONE',  ( -0.000000000000000000, -1.000000000000000000, -0.000000000000000000 ) ) ;
#7759 = CARTESIAN_POINT ( 'NONE',  ( -1.553300858899106629, 0.06250000000000002776, 0.2500000000000002220 ) ) ;
#7760 = CARTESIAN_POINT ( 'NONE',  ( -2.298097038856278029, 13.62500000000000000, -1.201902961143720638 ) ) ;
#7761 = CARTESIAN_POINT ( 'NONE',  ( 3.249999999999998224, 14.31250000000000355, -2.153805922287439945 ) ) ;
#7762 = VERTEX_POINT ( 'NONE', #13846 ) ;
#7763 = CARTESIAN_POINT ( 'NONE',  ( -1.346194077712559389, 12.06250000000000000, -0.2500000000000002220 ) ) ;
#7764 = AXIS2_PLACEMENT_3D ( 'NONE', #4998, #9863, #9941 ) ;
#7765 = CARTESIAN_POINT ( 'NONE',  ( 9.953425949663817107, 12.69566228043988332, -44.13594640649452572 ) ) ;
#7766 = CARTESIAN_POINT ( 'NONE',  ( -6.486570821710966328, 2.500000000000000000, -108.2546719218867253 ) ) ;
#7767 = CARTESIAN_POINT ( 'NONE',  ( -0.3766621274091715987, 0.5000000000000000000, -0.1347136637304948981 ) ) ;
#7768 = CARTESIAN_POINT ( 'NONE',  ( -6.777586278698688460, 14.47993771880504177, -116.7594943224638087 ) ) ;
#7769 = AXIS2_PLACEMENT_3D ( 'NONE', #13920, #3318, #2234 ) ;
#7770 = DATE_TIME_ROLE ( 'creation_date' ) ;
#7771 = CARTESIAN_POINT ( 'NONE',  ( 13.03594997100189268, 12.49999999999999822, -125.1067209762342145 ) ) ;
#7772 = CARTESIAN_POINT ( 'NONE',  ( 22.27832475887074537, 0.09828479602143111449, -138.8103524520464873 ) ) ;
#7773 = EDGE_LOOP ( 'NONE', ( #7129, #14642, #8087, #12949 ) ) ;
#7774 = CARTESIAN_POINT ( 'NONE',  ( -3.249999999999999556, 4.312500000000000888, -4.846194077712557835 ) ) ;
#7775 = CYLINDRICAL_SURFACE ( 'NONE', #8978, 3.250000000000005329 ) ;
#7776 = CARTESIAN_POINT ( 'NONE',  ( 2.651650429449554203, 3.375000000000000444, -0.8483495705504471296 ) ) ;
#7777 = VERTEX_POINT ( 'NONE', #7959 ) ;
#7778 = DIRECTION ( 'NONE',  ( -0.000000000000000000, -1.000000000000000000, -0.000000000000000000 ) ) ;
#7779 = PERSON ( 'NAUO-PER8', 'UNSPECIFIED', 'UNSPECIFIED', ('UNSPECIFIED'), ('UNSPECIFIED'), ('UNSPECIFIED') ) ;
#7780 = CARTESIAN_POINT ( 'NONE',  ( 1.553300858899105963, 3.562500000000000444, -7.250000000000000888 ) ) ;
#7781 = EDGE_CURVE ( 'NONE', #2992, #14660, #12679, .T. ) ;
#7782 = EDGE_CURVE ( 'NONE', #7799, #13718, #14872, .T. ) ;
#7783 = CARTESIAN_POINT ( 'NONE',  ( 7.302490728567498479, 3.561478500444579698, -24.97446755075041125 ) ) ;
#7784 = CARTESIAN_POINT ( 'NONE',  ( 0.2568603580465786962, 4.429590276632575652, 2.909462025691655462 ) ) ;
#7785 = CARTESIAN_POINT ( 'NONE',  ( 2.651650429449553759, 0.8750000000000000000, -0.8483495705504471296 ) ) ;
#7786 = DATE_TIME_ROLE ( 'classification_date' ) ;
#7787 = ADVANCED_FACE ( 'NONE', ( #4190 ), #3028, .T. ) ;
#7788 = CARTESIAN_POINT ( 'NONE',  ( 10.00087860767147063, 5.000000000000000888, -45.95880046359209103 ) ) ;
#7789 = CARTESIAN_POINT ( 'NONE',  ( -2.298097038856278473, 11.12500000000000000, -1.201902961143720416 ) ) ;
#7790 = CARTESIAN_POINT ( 'NONE',  ( -7.439587717305479408, 0.000000000000000000, -35.49614290395457772 ) ) ;
#7791 = ORIENTED_EDGE ( 'NONE', *, *, #11038, .F. ) ;
#7792 = DIRECTION ( 'NONE',  ( -0.000000000000000000, -1.000000000000000000, -0.000000000000000000 ) ) ;
#7793 = CARTESIAN_POINT ( 'NONE',  ( -1.346194077712558945, 3.562500000000000888, -0.2500000000000002220 ) ) ;
#7794 = DIRECTION ( 'NONE',  ( -0.9999404825435597166, 0.000000000000000000, -0.01091014988682699645 ) ) ;
#7795 = DIRECTION ( 'NONE',  ( -0.7220210382022110851, 0.000000000000000000, 0.6918711009959885860 ) ) ;
#7796 = CARTESIAN_POINT ( 'NONE',  ( 2.651650429449552870, 7.124999999999999112, -6.151650429449553314 ) ) ;
#7797 = CARTESIAN_POINT ( 'NONE',  ( -1.553300858899107073, 8.437500000000000000, -7.250000000000000000 ) ) ;
#7798 = CARTESIAN_POINT ( 'NONE',  ( -2.987892022880174636, 2.410101856083632477, -1.000000000000001110 ) ) ;
#7799 = VERTEX_POINT ( 'NONE', #10059 ) ;
#7800 = DIRECTION ( 'NONE',  ( -0.000000000000000000, -1.000000000000000000, -0.000000000000000000 ) ) ;
#7801 = CARTESIAN_POINT ( 'NONE',  ( 3.750000000000000000, 9.312500000000000000, -1.946699141100892705 ) ) ;
#7802 = CARTESIAN_POINT ( 'NONE',  ( 6.362474834385803746, 0.000000000000000000, -108.4026488224344291 ) ) ;
#7803 = CARTESIAN_POINT ( 'NONE',  ( -8.842600465860286363, -2.529993217055220178, -40.10276331981361864 ) ) ;
#7804 = ADVANCED_FACE ( 'NONE', ( #11218 ), #4268, .T. ) ;
#7805 = CARTESIAN_POINT ( 'NONE',  ( 33.75578156417349618, 0.000000000000000000, 39.47650855366864420 ) ) ;
#7806 = ORIENTED_EDGE ( 'NONE', *, *, #2241, .T. ) ;
#7807 = CARTESIAN_POINT ( 'NONE',  ( -22.54029179744063782, 8.673617379884035472E-16, -176.6655142756330861 ) ) ;
#7808 = CARTESIAN_POINT ( 'NONE',  ( 2.159942170319879562, 0.000000000000000000, -121.5147849362692369 ) ) ;
#7809 = CARTESIAN_POINT ( 'NONE',  ( -42.39238649434224726, 15.00000000000000000, -152.9358431397373863 ) ) ;
#7810 = CARTESIAN_POINT ( 'NONE',  ( -3.249999999999999112, 3.687500000000000444, -2.153805922287440833 ) ) ;
#7811 = ORIENTED_EDGE ( 'NONE', *, *, #14894, .F. ) ;
#7812 = LINE ( 'NONE', #2245, #4548 ) ;
#7813 = DIRECTION ( 'NONE',  ( 0.000000000000000000, 0.000000000000000000, 1.000000000000000000 ) ) ;
#7814 = CARTESIAN_POINT ( 'NONE',  ( -3.331919393530990092, 10.52300174851617953, -44.71933215806485151 ) ) ;
#7815 = CARTESIAN_POINT ( 'NONE',  ( -13.50165587222837438, 8.673617379884035472E-16, -183.0027181781699142 ) ) ;
#7816 = CARTESIAN_POINT ( 'NONE',  ( -3.504378794278709019, 8.673617379884035472E-16, -116.8541096786256333 ) ) ;
#7817 = CARTESIAN_POINT ( 'NONE',  ( -3.249999999999999556, 9.750000000000000000, -3.500000000000000000 ) ) ;
#7818 = CARTESIAN_POINT ( 'NONE',  ( 7.000000000000000888, 9.999999999999998224, -1.663700395152567513 ) ) ;
#7819 = CARTESIAN_POINT ( 'NONE',  ( 1.553300858899108849, 12.93750000000000000, 0.2499999999999993616 ) ) ;
#7820 = CARTESIAN_POINT ( 'NONE',  ( -63.59489740953759451, 14.99999999999999822, -201.2970526385593644 ) ) ;
#7821 = CARTESIAN_POINT ( 'NONE',  ( -7.876768715742058724, 13.10813300872041154, -104.9763684901371050 ) ) ;
#7822 = CARTESIAN_POINT ( 'NONE',  ( -2.298097038856278918, 13.37500000000000000, -5.798097038856277585 ) ) ;
#7823 =( BOUNDED_SURFACE ( )  B_SPLINE_SURFACE ( 3, 2, ( 
 ( #7537, #4149, #14821 ),
 ( #12323, #5229, #1742 ),
 ( #14672, #4077, #10164 ),
 ( #7688, #13509, #738 ),
 ( #666, #2905, #5445 ),
 ( #6452, #591, #5303 ),
 ( #5373, #2046, #7914 ),
 ( #6758, #9077, #9000 ),
 ( #7840, #13797, #12634 ),
 ( #8134, #10242, #891 ),
 ( #6980, #7988, #11696 ),
 ( #6827, #4368, #6898 ),
 ( #11620, #15045, #12710 ),
 ( #11473, #13727, #5664 ),
 ( #5593, #11543, #3127 ),
 ( #10307, #15200, #3275 ),
 ( #12863, #5817, #4518 ),
 ( #12556, #15124, #3197 ) ),
 .UNSPECIFIED., .F., .F., .T. ) 
 B_SPLINE_SURFACE_WITH_KNOTS ( ( 4, 2, 2, 2, 2, 2, 2, 2, 4 ),
 ( 3, 3 ),
 ( -1.470352482839513217E-05, 0.001632328272403186327, 0.002455844171018977187, 0.003279360069634767831, 0.004102875968250558475, 0.004514633917558453363, 0.004926391866866349119, 0.005749907765482139763, 0.006573423664097930406 ),
 ( 0.000000000000000000, 1.000000000000000000 ),
 .UNSPECIFIED. ) 
 GEOMETRIC_REPRESENTATION_ITEM ( )  RATIONAL_B_SPLINE_SURFACE ( (
 ( 1.000000000000000000, 1.000000000000000000, 1.000000000000000000),
 ( 1.000000000000000000, 1.000008545743839683, 1.000000000000000000),
 ( 1.000000000000000000, 0.9960198085043022731, 1.000000000000000000),
 ( 1.000000000000000000, 0.9835033616513570998, 1.000000000000000000),
 ( 1.000000000000000000, 0.9783561813779146910, 1.000000000000000000),
 ( 1.000000000000000000, 0.9664106271237844492, 1.000000000000000000),
 ( 1.000000000000000000, 0.9595652232277900318, 1.000000000000000000),
 ( 1.000000000000000000, 0.9448633500193042156, 1.000000000000000000),
 ( 1.000000000000000000, 0.9371864357976944504, 1.000000000000000000),
 ( 1.000000000000000000, 0.9259039669434644404, 1.000000000000000000),
 ( 1.000000000000000000, 0.9221838447129829808, 1.000000000000000000),
 ( 1.000000000000000000, 0.9149767654785520010, 1.000000000000000000),
 ( 1.000000000000000000, 0.9114704760577250209, 1.000000000000000000),
 ( 1.000000000000000000, 0.9018026765161173408, 1.000000000000000000),
 ( 1.000000000000000000, 0.8964349246879487199, 1.000000000000000000),
 ( 1.000000000000000000, 0.8889503419939598361, 1.000000000000000000),
 ( 1.000000000000000000, 0.8868438094748841705, 1.000000000000000000),
 ( 1.000000000000000000, 0.8868705507870419114, 1.000000000000000000) ) ) 
 REPRESENTATION_ITEM ( '' )  SURFACE ( )  );
#7824 = EDGE_CURVE ( 'NONE', #6005, #4454, #9700, .T. ) ;
#7825 = CARTESIAN_POINT ( 'NONE',  ( -65.53364736412717662, 5.000000000000000000, -205.7441351029432894 ) ) ;
#7826 = CARTESIAN_POINT ( 'NONE',  ( 4.912189190728483368, 14.88796584897967890, -1.019724683141319810 ) ) ;
#7827 = CARTESIAN_POINT ( 'NONE',  ( -1.346194077712559389, 9.437500000000000000, -6.749999999999999112 ) ) ;
#7828 = CARTESIAN_POINT ( 'NONE',  ( 2.891442464128509027, 0.5021605422368213834, 2.425309775607110030 ) ) ;
#7829 = CARTESIAN_POINT ( 'NONE',  ( -3.955596480971199203, 2.500000000000000000, -118.5438621456188173 ) ) ;
#7830 = ORIENTED_EDGE ( 'NONE', *, *, #3869, .F. ) ;
#7831 =( BOUNDED_SURFACE ( )  B_SPLINE_SURFACE ( 3, 2, ( 
 ( #12074, #13331, #3976 ),
 ( #1345, #2738, #182 ),
 ( #1498, #7442, #3735 ),
 ( #12158, #6288, #7520 ),
 ( #419, #5129, #9842 ),
 ( #8681, #1421, #13415 ),
 ( #6047, #2818, #4894 ),
 ( #1264, #10689, #9533 ) ),
 .UNSPECIFIED., .F., .F., .F. ) 
 B_SPLINE_SURFACE_WITH_KNOTS ( ( 4, 2, 2, 4 ),
 ( 3, 3 ),
 ( 0.04393710950295283413, 0.04951918683847043867, 0.05231022550622924094, 0.05510126417398804322 ),
 ( 0.000000000000000000, 1.000000000000000000 ),
 .UNSPECIFIED. ) 
 GEOMETRIC_REPRESENTATION_ITEM ( )  RATIONAL_B_SPLINE_SURFACE ( (
 ( 1.000000000000000000, 0.7071067811865473507, 1.000000000000000000),
 ( 1.000000000000000000, 0.7071067811865473507, 1.000000000000000000),
 ( 1.000000000000000000, 0.7071067811865471286, 1.000000000000000000),
 ( 1.000000000000000000, 0.7071067811865471286, 1.000000000000000000),
 ( 1.000000000000000000, 0.7071067811865476838, 1.000000000000000000),
 ( 1.000000000000000000, 0.7071067811865476838, 1.000000000000000000),
 ( 1.000000000000000000, 0.7071067811865473507, 1.000000000000000000),
 ( 1.000000000000000000, 0.7071067811865473507, 1.000000000000000000) ) ) 
 REPRESENTATION_ITEM ( '' )  SURFACE ( )  );
#7832 = DIRECTION ( 'NONE',  ( -0.000000000000000000, -1.000000000000000000, -0.000000000000000000 ) ) ;
#7833 = CARTESIAN_POINT ( 'NONE',  ( 2.469015410240005703, 15.00000000000000000, -109.2094522964932679 ) ) ;
#7834 = CARTESIAN_POINT ( 'NONE',  ( 1.553300858899105963, 2.562500000000000444, -7.250000000000000888 ) ) ;
#7835 = CARTESIAN_POINT ( 'NONE',  ( 0.000000000000000000, 15.50000000000000178, -0.2500000000000002220 ) ) ;
#7836 = CARTESIAN_POINT ( 'NONE',  ( -3.980102097228897245E-16, 1.500000000000000000, -6.749999999999999112 ) ) ;
#7837 = ORIENTED_EDGE ( 'NONE', *, *, #14807, .F. ) ;
#7838 = CARTESIAN_POINT ( 'NONE',  ( 3.249999999999999112, 11.81249999999999822, -2.153805922287439945 ) ) ;
#7839 = LINE ( 'NONE', #5302, #9150 ) ;
#7840 = CARTESIAN_POINT ( 'NONE',  ( -7.848833331099569044, 13.14512866485396181, -104.9618519593132078 ) ) ;
#7841 = PLANE ( 'NONE',  #3008 ) ;
#7842 = CARTESIAN_POINT ( 'NONE',  ( -9.392097536374429012, 11.74640706408357005, -116.4406435548276022 ) ) ;
#7843 = PERSON_AND_ORGANIZATION_ROLE ( 'design_supplier' ) ;
#7844 = CARTESIAN_POINT ( 'NONE',  ( 11.86796838824852607, 12.49999999999999822, -123.5172601093923248 ) ) ;
#7845 = DIRECTION ( 'NONE',  ( 0.000000000000000000, -0.000000000000000000, 1.000000000000000000 ) ) ;
#7846 = CARTESIAN_POINT ( 'NONE',  ( 25.97495963226450755, 1.795150172152642165, -137.7704446659557220 ) ) ;
#7847 = ORIENTED_EDGE ( 'NONE', *, *, #13250, .T. ) ;
#7848 = CARTESIAN_POINT ( 'NONE',  ( -3.980102097228897245E-16, 6.500000000000000888, -6.749999999999999112 ) ) ;
#7849 = CARTESIAN_POINT ( 'NONE',  ( -23.62092208418379258, 4.000000000000000888, -167.0316697996453286 ) ) ;
#7850 = CARTESIAN_POINT ( 'NONE',  ( -1.553300858899106629, 3.562500000000000888, 0.2500000000000002220 ) ) ;
#7851 = ORIENTED_EDGE ( 'NONE', *, *, #1020, .T. ) ;
#7852 = CARTESIAN_POINT ( 'NONE',  ( -4.561986575595136983, 15.00000000000000355, -117.3660065143356235 ) ) ;
#7853 = CARTESIAN_POINT ( 'NONE',  ( -1.553300858899107295, 7.437500000000000888, -7.250000000000000000 ) ) ;
#7854 = CARTESIAN_POINT ( 'NONE',  ( 7.781170200712294260, 5.000000000000000888, -20.49502329017444424 ) ) ;
#7855 = CARTESIAN_POINT ( 'NONE',  ( 0.2483469068648843925, 4.114088372968399021, 2.813030006718263643 ) ) ;
#7856 = CARTESIAN_POINT ( 'NONE',  ( -3.750000000000000000, 3.187500000000000444, -1.946699141100892927 ) ) ;
#7857 = SECURITY_CLASSIFICATION_LEVEL ( 'unclassified' ) ;
#7858 = FACE_OUTER_BOUND ( 'NONE', #1560, .T. ) ;
#7859 = DIRECTION ( 'NONE',  ( 0.08794243244723021213, 0.000000000000000000, 0.9961255586397049777 ) ) ;
#7860 = VERTEX_POINT ( 'NONE', #1636 ) ;
#7861 = CARTESIAN_POINT ( 'NONE',  ( -3.249999999999999112, 2.812500000000000444, -4.846194077712558723 ) ) ;
#7862 = ADVANCED_FACE ( 'NONE', ( #8896 ), #12144, .F. ) ;
#7863 = DIRECTION ( 'NONE',  ( 0.02693067314564481438, -0.8090169943749466741, -0.5871679841888947093 ) ) ;
#7864 = CARTESIAN_POINT ( 'NONE',  ( 2.651650429449553314, 8.375000000000000000, -0.8483495705504476847 ) ) ;
#7865 = CARTESIAN_POINT ( 'NONE',  ( -1.553300858899106407, 13.06250000000000000, 0.2500000000000002220 ) ) ;
#7866 = DIRECTION ( 'NONE',  ( 0.000000000000000000, -0.000000000000000000, 1.000000000000000000 ) ) ;
#7867 = CARTESIAN_POINT ( 'NONE',  ( 4.030605408878806806, -2.051692149507289097E-14, 7.295648618995384638 ) ) ;
#7868 = CARTESIAN_POINT ( 'NONE',  ( -2.651650429449552870, 9.624999999999998224, -0.8483495705504463524 ) ) ;
#7869 = CARTESIAN_POINT ( 'NONE',  ( 4.916379274077837813, 14.85715077789358673, -0.5990194345177435320 ) ) ;
#7870 = ADVANCED_FACE ( 'NONE', ( #5415 ), #7579, .T. ) ;
#7871 = CARTESIAN_POINT ( 'NONE',  ( 26.17093350124943640, 6.000000000000000000, -137.7213801722282085 ) ) ;
#7872 = DIRECTION ( 'NONE',  ( 0.000000000000000000, 1.000000000000000000, 0.000000000000000000 ) ) ;
#7873 = ORIENTED_EDGE ( 'NONE', *, *, #13873, .F. ) ;
#7874 = CARTESIAN_POINT ( 'NONE',  ( -15.33183641037303069, -1.091572321461162701E-12, -155.5537725507397795 ) ) ;
#7875 = CARTESIAN_POINT ( 'NONE',  ( -51.02532656535751698, 9.999999999999998224, -166.3766172518998587 ) ) ;
#7876 = CARTESIAN_POINT ( 'NONE',  ( 3.249999999999999556, 3.250000000000000000, -3.500000000000000000 ) ) ;
#7877 = EDGE_LOOP ( 'NONE', ( #10173, #4085, #2087, #3890, #8162 ) ) ;
#7878 = CARTESIAN_POINT ( 'NONE',  ( 7.101058424337646890, 5.000000000000000888, -131.4073749499507642 ) ) ;
#7879 = CARTESIAN_POINT ( 'NONE',  ( 0.7644969749118040170, 5.000000000000000000, -138.4027240657576101 ) ) ;
#7880 = CARTESIAN_POINT ( 'NONE',  ( -8.272624645278304101, 14.99999999999999822, -140.4230430975193258 ) ) ;
#7881 = SECURITY_CLASSIFICATION ( '', '', #8851 ) ;
#7882 = CARTESIAN_POINT ( 'NONE',  ( 6.447361309400962526, 15.00000000000000000, 0.5877790035379841793 ) ) ;
#7883 = EDGE_CURVE ( 'NONE', #1674, #6652, #7735, .T. ) ;
#7884 = CARTESIAN_POINT ( 'NONE',  ( 3.743303269468425842, 8.673617379884035472E-16, -106.5640776127142004 ) ) ;
#7885 = CARTESIAN_POINT ( 'NONE',  ( 3.249999999999999556, 10.25000000000000178, -3.500000000000000000 ) ) ;
#7886 = AXIS2_PLACEMENT_3D ( 'NONE', #452, #13447, #7621 ) ;
#7887 = CARTESIAN_POINT ( 'NONE',  ( 24.53888684075855409, 5.000000000000000888, -142.6514391812075928 ) ) ;
#7888 = CARTESIAN_POINT ( 'NONE',  ( 2.651650429449553759, 12.87500000000000178, -0.8483495705504471296 ) ) ;
#7889 = LINE ( 'NONE', #14729, #12356 ) ;
#7890 = CARTESIAN_POINT ( 'NONE',  ( 1.756204145886661516, 2.540697700117988678, -1.000000000000001110 ) ) ;
#7891 = CARTESIAN_POINT ( 'NONE',  ( -2.298097038856278473, 12.12500000000000000, -1.201902961143720416 ) ) ;
#7892 = CARTESIAN_POINT ( 'NONE',  ( 20.87131526946579285, 0.000000000000000000, -138.9752963459259547 ) ) ;
#7893 = CC_DESIGN_SECURITY_CLASSIFICATION ( #10865, ( #15324 ) ) ;
#7894 = PLANE ( 'NONE',  #4319 ) ;
#7895 = CARTESIAN_POINT ( 'NONE',  ( 1.346194077712558057, 10.56250000000000000, -6.750000000000000000 ) ) ;
#7896 = AXIS2_PLACEMENT_3D ( 'NONE', #9153, #4295, #13878 ) ;
#7897 = CARTESIAN_POINT ( 'NONE',  ( 26.58801926426209405, 6.000000000000000000, -139.0072983920785532 ) ) ;
#7898 = ORIENTED_EDGE ( 'NONE', *, *, #6495, .F. ) ;
#7899 = ORIENTED_EDGE ( 'NONE', *, *, #5428, .F. ) ;
#7900 = CARTESIAN_POINT ( 'NONE',  ( 3.558820106718695975, 15.00000000000000000, -107.0002797207564242 ) ) ;
#7901 = CARTESIAN_POINT ( 'NONE',  ( -4.592425496802573972E-16, 2.500000000000000000, -7.249999999999999112 ) ) ;
#7902 = CARTESIAN_POINT ( 'NONE',  ( 2.651650429449552870, 1.124999999999999778, -6.151650429449553314 ) ) ;
#7903 = CARTESIAN_POINT ( 'NONE',  ( 26.58801926426209405, 5.000000000000000888, -139.0072983920785532 ) ) ;
#7904 = ORIENTED_EDGE ( 'NONE', *, *, #10640, .T. ) ;
#7905 = ADVANCED_FACE ( 'NONE', ( #4120 ), #13478, .F. ) ;
#7906 = CARTESIAN_POINT ( 'NONE',  ( -3.249999999999999556, 12.31250000000000000, -4.846194077712557835 ) ) ;
#7907 = ADVANCED_FACE ( 'NONE', ( #6275 ), #12373, .F. ) ;
#7908 = ADVANCED_FACE ( 'NONE', ( #10990, #11141 ), #6422, .F. ) ;
#7909 = AXIS2_PLACEMENT_3D ( 'NONE', #9610, #15207, #13022 ) ;
#7910 =( BOUNDED_SURFACE ( )  B_SPLINE_SURFACE ( 3, 1, ( 
 ( #9844, #14577 ),
 ( #3312, #9411 ),
 ( #4473, #4397 ),
 ( #3231, #9183 ) ),
 .UNSPECIFIED., .F., .F., .F. ) 
 B_SPLINE_SURFACE_WITH_KNOTS ( ( 4, 4 ),
 ( 2, 2 ),
 ( 0.000000000000000000, 1.000000000000000000 ),
 ( 0.000000000000000000, 1.000000000000000000 ),
 .UNSPECIFIED. ) 
 GEOMETRIC_REPRESENTATION_ITEM ( )  RATIONAL_B_SPLINE_SURFACE ( (
 ( 1.000000000000000000, 1.000000000000000000),
 ( 0.6468719831415912225, 0.6468719831415912225),
 ( 0.6468719831415912225, 0.6468719831415912225),
 ( 1.000000000000000000, 1.000000000000000000) ) ) 
 REPRESENTATION_ITEM ( '' )  SURFACE ( )  );
#7911 = CARTESIAN_POINT ( 'NONE',  ( -3.648797883638980277, -2.490287375297125294, -1.000000000000000888 ) ) ;
#7912 = AXIS2_PLACEMENT_3D ( 'NONE', #589, #8999, #9076 ) ;
#7913 = AXIS2_PLACEMENT_3D ( 'NONE', #11264, #8633, #1847 ) ;
#7914 = CARTESIAN_POINT ( 'NONE',  ( -7.398019396816514437, 13.84373920337187691, -104.1012393012796764 ) ) ;
#7915 = FACE_OUTER_BOUND ( 'NONE', #4619, .T. ) ;
#7916 = CC_DESIGN_PERSON_AND_ORGANIZATION_ASSIGNMENT ( #4997, #2761, ( #9370 ) ) ;
#7917 = APPROVAL_ROLE ( '' ) ;
#7918 = CARTESIAN_POINT ( 'NONE',  ( 5.957819783299798111, 15.00000000000000000, -111.9092042284245707 ) ) ;
#7919 = CARTESIAN_POINT ( 'NONE',  ( -9.410661088365813498, 11.69876074752964712, -116.4362230898866386 ) ) ;
#7920 = ORIENTED_EDGE ( 'NONE', *, *, #8092, .F. ) ;
#7921 = CARTESIAN_POINT ( 'NONE',  ( 24.27947087742526833, 0.8297099930049451899, -138.5673885577481883 ) ) ;
#7922 = CARTESIAN_POINT ( 'NONE',  ( -2.298097038856278473, 11.12500000000000000, -1.201902961143720416 ) ) ;
#7923 = VECTOR ( 'NONE', #11974, 1000.000000000000000 ) ;
#7924 = EDGE_LOOP ( 'NONE', ( #2092, #1123 ) ) ;
#7925 = CIRCLE ( 'NONE', #5456, 0.5000000000000001110 ) ;
#7926 = CARTESIAN_POINT ( 'NONE',  ( 0.000000000000000000, 6.000000000000000000, -0.2500000000000002220 ) ) ;
#7927 = CARTESIAN_POINT ( 'NONE',  ( -8.289881740238502772, -2.075239479414269894, -35.21986562831451550 ) ) ;
#7928 = CARTESIAN_POINT ( 'NONE',  ( -1.553300858899106629, 1.562500000000000222, 0.2500000000000002220 ) ) ;
#7929 = EDGE_LOOP ( 'NONE', ( #4828, #6112, #7082, #5583 ) ) ;
#7930 = CARTESIAN_POINT ( 'NONE',  ( 1.500000000000000000, 4.500000000000000888, -0.2499999999999997780 ) ) ;
#7931 = CARTESIAN_POINT ( 'NONE',  ( 2.298097038856278473, 0.6250000000000000000, -5.798097038856279362 ) ) ;
#7932 = CARTESIAN_POINT ( 'NONE',  ( 2.651650429449553759, 3.875000000000000000, -0.8483495705504471296 ) ) ;
#7933 = AXIS2_PLACEMENT_3D ( 'NONE', #14232, #12994, #3403 ) ;
#7934 = CARTESIAN_POINT ( 'NONE',  ( -25.35797282612971770, 0.03589225196800699402, -200.8427820752426953 ) ) ;
#7935 = CARTESIAN_POINT ( 'NONE',  ( -0.3545318111937544869, 10.00000000000000178, -139.6177279649697596 ) ) ;
#7936 = DATE_TIME_ROLE ( 'creation_date' ) ;
#7937 = CARTESIAN_POINT ( 'NONE',  ( -37.86885108244810283, 15.00000000000000000, -139.8897182464016566 ) ) ;
#7938 = FACE_OUTER_BOUND ( 'NONE', #11551, .T. ) ;
#7939 = ORIENTED_EDGE ( 'NONE', *, *, #11781, .F. ) ;
#7940 = CARTESIAN_POINT ( 'NONE',  ( 0.000000000000000000, 1.500000000000000222, -0.2500000000000002220 ) ) ;
#7941 = CARTESIAN_POINT ( 'NONE',  ( 10.81798288406372421, 13.62122652546089618, -106.9829802339604612 ) ) ;
#7942 = CARTESIAN_POINT ( 'NONE',  ( 3.749999999999998668, 8.187500000000000000, -5.053300858899108405 ) ) ;
#7943 = CARTESIAN_POINT ( 'NONE',  ( 2.651650429449552870, 14.62500000000000000, -6.151650429449554203 ) ) ;
#7944 = CARTESIAN_POINT ( 'NONE',  ( -64.87526564358481096, 14.94604455467652571, -187.2214054586863483 ) ) ;
#7945 = ORIENTED_EDGE ( 'NONE', *, *, #834, .F. ) ;
#7946 = LINE ( 'NONE', #4179, #14112 ) ;
#7947 = CARTESIAN_POINT ( 'NONE',  ( 0.000000000000000000, 13.50000000000000178, 0.2500000000000002220 ) ) ;
#7948 = DIRECTION ( 'NONE',  ( 0.000000000000000000, 0.000000000000000000, 1.000000000000000000 ) ) ;
#7949 = PERSON_AND_ORGANIZATION_ROLE ( 'design_owner' ) ;
#7950 = SECURITY_CLASSIFICATION ( '', '', #6514 ) ;
#7951 = LINE ( 'NONE', #12593, #6041 ) ;
#7952 = VERTEX_POINT ( 'NONE', #5195 ) ;
#7953 = CARTESIAN_POINT ( 'NONE',  ( -24.35736811731606366, 8.673617379884035472E-16, -201.5239328345637091 ) ) ;
#7954 = CARTESIAN_POINT ( 'NONE',  ( -3.249999999999999556, 0.1874999999999999722, -2.153805922287440833 ) ) ;
#7955 = CARTESIAN_POINT ( 'NONE',  ( -42.37771161479906112, 15.00000000000000000, -158.4861704486624774 ) ) ;
#7956 = CARTESIAN_POINT ( 'NONE',  ( -1.346194077712559167, 1.937500000000000222, -6.749999999999999112 ) ) ;
#7957 = ORIENTED_EDGE ( 'NONE', *, *, #2330, .F. ) ;
#7958 = CARTESIAN_POINT ( 'NONE',  ( -11.40820045156521623, 15.00000000000000000, -126.3212311507313217 ) ) ;
#7959 = CARTESIAN_POINT ( 'NONE',  ( -8.351752737786036107, 9.999999999999998224, -94.60045770897244211 ) ) ;
#7960 = LINE ( 'NONE', #2096, #3806 ) ;
#7961 = CARTESIAN_POINT ( 'NONE',  ( 6.277464105443620213, 14.50508960634419431, 2.466953552936270277 ) ) ;
#7962 = CARTESIAN_POINT ( 'NONE',  ( -1.030030362070360139, 8.673617379884035472E-16, -105.0143096063716399 ) ) ;
#7963 = CARTESIAN_POINT ( 'NONE',  ( -2.298097038856279362, 13.87500000000000178, -5.798097038856278473 ) ) ;
#7964 = CARTESIAN_POINT ( 'NONE',  ( 0.000000000000000000, 4.000000000000000000, -2.000000000000000000 ) ) ;
#7965 = CARTESIAN_POINT ( 'NONE',  ( -2.651650429449553314, 3.875000000000000444, -6.151650429449552426 ) ) ;
#7966 = AXIS2_PLACEMENT_3D ( 'NONE', #12351, #2783, #11117 ) ;
#7967 = DIRECTION ( 'NONE',  ( -0.02032500363964214948, 0.3636704086172903305, 0.9313059261720508797 ) ) ;
#7968 = CARTESIAN_POINT ( 'NONE',  ( -4.716550020523635922, 14.96884535972561103, -103.4640810165829237 ) ) ;
#7969 = CARTESIAN_POINT ( 'NONE',  ( -0.3732829694918187724, 15.00000000000000000, -108.7490593617764461 ) ) ;
#7970 = DIRECTION ( 'NONE',  ( -0.9961255586397056438, -0.000000000000000000, 0.08794243244722427244 ) ) ;
#7971 = EDGE_CURVE ( 'NONE', #12098, #3600, #13151, .T. ) ;
#7972 = CARTESIAN_POINT ( 'NONE',  ( -2.357250054738958767, 2.100000000000253664, -0.4319429197694263367 ) ) ;
#7973 = CARTESIAN_POINT ( 'NONE',  ( 3.249999999999999112, 8.812500000000000000, -2.153805922287439945 ) ) ;
#7974 = CARTESIAN_POINT ( 'NONE',  ( -7.234633885585873614, 5.000000000000000888, -146.9955140158000404 ) ) ;
#7975 = APPLICATION_CONTEXT ( 'configuration controlled 3d designs of mechanical parts and assemblies' ) ;
#7976 = CARTESIAN_POINT ( 'NONE',  ( -49.91314714375069173, 0.000000000000000000, -125.9106517931341500 ) ) ;
#7977 = EDGE_LOOP ( 'NONE', ( #1139, #984, #2435, #10987 ) ) ;
#7978 = ORIENTED_EDGE ( 'NONE', *, *, #15306, .F. ) ;
#7979 = DIRECTION ( 'NONE',  ( 0.000000000000000000, 0.000000000000000000, 1.000000000000000000 ) ) ;
#7980 = CARTESIAN_POINT ( 'NONE',  ( -1.553300858899107295, 2.437500000000000444, -7.250000000000000000 ) ) ;
#7981 = AXIS2_PLACEMENT_3D ( 'NONE', #9527, #13321, #3889 ) ;
#7982 = CARTESIAN_POINT ( 'NONE',  ( 3.249999999999998224, 14.31250000000000355, -2.153805922287439945 ) ) ;
#7983 = AXIS2_PLACEMENT_3D ( 'NONE', #9165, #7696, #6838 ) ;
#7984 = CARTESIAN_POINT ( 'NONE',  ( 5.079523875935373134, 9.999999999999998224, -108.2552591983082806 ) ) ;
#7985 = ORIENTED_EDGE ( 'NONE', *, *, #12426, .T. ) ;
#7986 = CARTESIAN_POINT ( 'NONE',  ( 3.249999999999999112, 14.81250000000000000, -2.153805922287439945 ) ) ;
#7987 = DIRECTION ( 'NONE',  ( 0.000000000000000000, 0.000000000000000000, -1.000000000000000000 ) ) ;
#7988 = CARTESIAN_POINT ( 'NONE',  ( -8.470420019481499807, 12.69254319550381283, -104.8380799168281214 ) ) ;
#7989 = CARTESIAN_POINT ( 'NONE',  ( 3.249999999999999556, 3.750000000000000000, -3.500000000000000000 ) ) ;
#7990 = VECTOR ( 'NONE', #7778, 1000.000000000000000 ) ;
#7991 = APPROVAL_ROLE ( '' ) ;
#7992 = AXIS2_PLACEMENT_3D ( 'NONE', #406, #9830, #14562 ) ;
#7993 = EDGE_CURVE ( 'NONE', #9274, #447, #9193, .T. ) ;
#7994 = CARTESIAN_POINT ( 'NONE',  ( 8.308576004039894158, 12.49999999999999822, -113.5907613746754379 ) ) ;
#7995 = CYLINDRICAL_SURFACE ( 'NONE', #10600, 2.500000000000000000 ) ;
#7996 = ORIENTED_EDGE ( 'NONE', *, *, #1604, .T. ) ;
#7997 = EDGE_CURVE ( 'NONE', #7183, #887, #9909, .T. ) ;
#7998 = CARTESIAN_POINT ( 'NONE',  ( 25.22353789337514129, 1.212876488842051792, -137.9529182181685201 ) ) ;
#7999 = CARTESIAN_POINT ( 'NONE',  ( -3.980102097228897245E-16, 12.50000000000000000, -6.749999999999999112 ) ) ;
#8000 = ORIENTED_EDGE ( 'NONE', *, *, #3922, .F. ) ;
#8001 = ORIENTED_EDGE ( 'NONE', *, *, #1205, .T. ) ;
#8002 = CARTESIAN_POINT ( 'NONE',  ( -3.249999999999999556, 3.187500000000000000, -2.153805922287440833 ) ) ;
#8003 = CARTESIAN_POINT ( 'NONE',  ( -2.651650429449552870, 1.625000000000000000, -0.8483495705504463524 ) ) ;
#8004 = CARTESIAN_POINT ( 'NONE',  ( 1.346194077712558279, 7.062500000000000888, -6.750000000000000888 ) ) ;
#8005 = ORIENTED_EDGE ( 'NONE', *, *, #11002, .F. ) ;
#8006 = CARTESIAN_POINT ( 'NONE',  ( -5.609161682253958503, 1.749999999999405365, 27.59976306049381378 ) ) ;
#8007 = DIRECTION ( 'NONE',  ( -0.000000000000000000, -1.000000000000000000, -0.000000000000000000 ) ) ;
#8008 = CARTESIAN_POINT ( 'NONE',  ( 1.553300858899108849, 4.937500000000001776, 0.2499999999999993616 ) ) ;
#8009 = CARTESIAN_POINT ( 'NONE',  ( -25.05565439364611535, 2.706536666467781682, -208.8267152099942621 ) ) ;
#8010 = CARTESIAN_POINT ( 'NONE',  ( -13.68460728451510633, 7.499999999999991118, -92.46488696946715891 ) ) ;
#8011 = APPLICATION_PROTOCOL_DEFINITION ( 'international standard', 'config_control_design', 1994, #7975 ) ;
#8012 = CARTESIAN_POINT ( 'NONE',  ( 9.697215460253069352, 5.000000000000000000, -119.7729938534562564 ) ) ;
#8013 = AXIS2_PLACEMENT_3D ( 'NONE', #5429, #14734, #2961 ) ;
#8014 = EDGE_CURVE ( 'NONE', #8185, #7526, #13659, .T. ) ;
#8015 = VERTEX_POINT ( 'NONE', #13549 ) ;
#8016 = CARTESIAN_POINT ( 'NONE',  ( 2.298097038856278029, 8.125000000000000000, -5.798097038856279362 ) ) ;
#8017 = CARTESIAN_POINT ( 'NONE',  ( 11.32016196459912649, 5.000000000000000888, -106.4092894470390291 ) ) ;
#8018 = AXIS2_PLACEMENT_3D ( 'NONE', #2011, #15164, #12670 ) ;
#8019 = CARTESIAN_POINT ( 'NONE',  ( 3.749999999999999112, 9.312500000000001776, -1.946699141100893149 ) ) ;
#8020 = CARTESIAN_POINT ( 'NONE',  ( -33.91109452335874153, 5.000000000000000000, -156.1716796081737471 ) ) ;
#8021 = CARTESIAN_POINT ( 'NONE',  ( -63.60348060676461301, 15.00000000000000000, -180.2685449772604329 ) ) ;
#8022 = ORIENTED_EDGE ( 'NONE', *, *, #13958, .T. ) ;
#8023 = DIRECTION ( 'NONE',  ( -8.764770998266003672E-18, -0.000000000000000000, -1.000000000000000000 ) ) ;
#8024 = CARTESIAN_POINT ( 'NONE',  ( -2.298097038856278473, 8.125000000000000000, -1.201902961143720416 ) ) ;
#8025 = CARTESIAN_POINT ( 'NONE',  ( 2.651650429449554203, 13.37500000000000000, -0.8483495705504471296 ) ) ;
#8026 = CARTESIAN_POINT ( 'NONE',  ( -2.893252786143252653, 4.336808689942017736E-16, -110.6524584094670445 ) ) ;
#8027 = DATE_TIME_ROLE ( 'creation_date' ) ;
#8028 = CARTESIAN_POINT ( 'NONE',  ( 9.952467559749662129, 4.873278229199302203, -43.74057228409819231 ) ) ;
#8029 = ORIENTED_EDGE ( 'NONE', *, *, #3454, .T. ) ;
#8030 = CARTESIAN_POINT ( 'NONE',  ( 8.935548306886577308, 4.740853562920613662, 2.855381321663926997 ) ) ;
#8031 = CARTESIAN_POINT ( 'NONE',  ( -1.346194077712559167, 0.4375000000000000000, -6.749999999999999112 ) ) ;
#8032 = CARTESIAN_POINT ( 'NONE',  ( -53.69697306021766536, 9.999999999999998224, -170.4167521506420258 ) ) ;
#8033 = CARTESIAN_POINT ( 'NONE',  ( -2.298097038856278029, 3.625000000000000888, -1.201902961143720638 ) ) ;
#8034 = ORIENTED_EDGE ( 'NONE', *, *, #797, .F. ) ;
#8035 = CARTESIAN_POINT ( 'NONE',  ( 7.220173501946012706, 9.999999999999996447, -111.8642345870615458 ) ) ;
#8036 = CARTESIAN_POINT ( 'NONE',  ( -25.48627911830238801, 3.148413055323376231, -208.6114731983374782 ) ) ;
#8037 = CARTESIAN_POINT ( 'NONE',  ( 6.172424634706433544, 13.06580985397910943, 4.242162613119662140 ) ) ;
#8038 = CARTESIAN_POINT ( 'NONE',  ( -5.318033920856502839, 5.000000000000000888, -111.4753907371883059 ) ) ;
#8039 = CARTESIAN_POINT ( 'NONE',  ( -2.298097038856279362, 12.87500000000000178, -5.798097038856278473 ) ) ;
#8040 = CARTESIAN_POINT ( 'NONE',  ( 12.80648593303889271, 8.673617379884035472E-16, -154.6494596161801098 ) ) ;
#8041 = CARTESIAN_POINT ( 'NONE',  ( -2.651650429449553314, 0.8750000000000000000, -6.151650429449552426 ) ) ;
#8042 = DIRECTION ( 'NONE',  ( -0.000000000000000000, 1.000000000000000000, -0.000000000000000000 ) ) ;
#8043 = CARTESIAN_POINT ( 'NONE',  ( -5.747484833204142163, 12.90644774961933372, -125.0474022778247587 ) ) ;
#8044 = CARTESIAN_POINT ( 'NONE',  ( 23.58041249293978581, 0.5629353006154804717, -138.0219903428570944 ) ) ;
#8045 = CARTESIAN_POINT ( 'NONE',  ( -0.3675725891509502574, 0.000000000000000000, -0.3389548520155299949 ) ) ;
#8046 = CARTESIAN_POINT ( 'NONE',  ( -2.298097038856278473, 8.125000000000000000, -1.201902961143720416 ) ) ;
#8047 = CARTESIAN_POINT ( 'NONE',  ( 3.891364641103943978, 14.90536770052034932, -1.768596708628486613 ) ) ;
#8048 = LINE ( 'NONE', #11385, #9622 ) ;
#8049 = ORIENTED_EDGE ( 'NONE', *, *, #365, .T. ) ;
#8050 = ORIENTED_EDGE ( 'NONE', *, *, #1280, .F. ) ;
#8051 = CARTESIAN_POINT ( 'NONE',  ( -14.35488426859573785, 8.673617379884035472E-16, -183.9742857961890081 ) ) ;
#8052 = CARTESIAN_POINT ( 'NONE',  ( -3.749999999999999556, 4.187500000000000000, -1.946699141100892927 ) ) ;
#8053 = CARTESIAN_POINT ( 'NONE',  ( -1.553300858899106629, 1.562500000000000222, 0.2499999999999998335 ) ) ;
#8054 = CARTESIAN_POINT ( 'NONE',  ( 38.58381714758451864, 1.749999999999999778, 41.14817863027235489 ) ) ;
#8055 = EDGE_LOOP ( 'NONE', ( #3956, #6872 ) ) ;
#8056 = ADVANCED_FACE ( 'NONE', ( #2949 ), #1790, .T. ) ;
#8057 = ADVANCED_FACE ( 'NONE', ( #11362 ), #934, .T. ) ;
#8058 = EDGE_CURVE ( 'NONE', #1120, #3740, #3035, .T. ) ;
#8059 = CARTESIAN_POINT ( 'NONE',  ( 2.298097038856278029, 1.124999999999999778, -5.798097038856279362 ) ) ;
#8060 = ADVANCED_FACE ( 'NONE', ( #9275 ), #13572, .F. ) ;
#8061 = CARTESIAN_POINT ( 'NONE',  ( -0.4453226528549816265, -2.225540348348185052E-17, 1.000000000000000000 ) ) ;
#8062 = VECTOR ( 'NONE', #11154, 1000.000000000000114 ) ;
#8063 = CARTESIAN_POINT ( 'NONE',  ( -13.86049214940955387, 7.499999999999991118, -94.45713808674658196 ) ) ;
#8064 = CARTESIAN_POINT ( 'NONE',  ( -3.249999999999999556, 4.312500000000000888, -4.846194077712557835 ) ) ;
#8065 = DATE_TIME_ROLE ( 'classification_date' ) ;
#8066 = CARTESIAN_POINT ( 'NONE',  ( 0.000000000000000000, 0.000000000000000000, 0.000000000000000000 ) ) ;
#8067 = DIRECTION ( 'NONE',  ( 0.000000000000000000, 1.000000000000000000, 0.000000000000000000 ) ) ;
#8068 = ORIENTED_EDGE ( 'NONE', *, *, #11581, .F. ) ;
#8069 = CARTESIAN_POINT ( 'NONE',  ( 26.44917159162123355, 3.476039578930857132, -136.9761077298000203 ) ) ;
#8070 = CARTESIAN_POINT ( 'NONE',  ( -1.346194077712558945, 9.062500000000000000, -0.2500000000000002220 ) ) ;
#8071 = ORIENTED_EDGE ( 'NONE', *, *, #11100, .F. ) ;
#8072 = ORIENTED_EDGE ( 'NONE', *, *, #11381, .F. ) ;
#8073 = CARTESIAN_POINT ( 'NONE',  ( -3.749999999999999556, 9.750000000000000000, -3.499999999999999112 ) ) ;
#8074 = FACE_OUTER_BOUND ( 'NONE', #11850, .T. ) ;
#8075 = CARTESIAN_POINT ( 'NONE',  ( 2.651650429449554203, 0.3750000000000001110, -0.8483495705504471296 ) ) ;
#8076 = CARTESIAN_POINT ( 'NONE',  ( -3.249999999999999112, 7.687500000000000888, -2.153805922287440833 ) ) ;
#8077 = EDGE_LOOP ( 'NONE', ( #3884, #901, #10381, #2360 ) ) ;
#8078 = DIRECTION ( 'NONE',  ( 0.6005713924789962688, 0.000000000000000000, -0.7995711366325319869 ) ) ;
#8079 = CARTESIAN_POINT ( 'NONE',  ( 1.346194077712560944, 4.937500000000001776, -0.2500000000000010547 ) ) ;
#8080 = CARTESIAN_POINT ( 'NONE',  ( -3.749999999999999556, 7.312500000000000888, -5.053300858899104853 ) ) ;
#8081 = EDGE_CURVE ( 'NONE', #4358, #3762, #11663, .T. ) ;
#8082 = CARTESIAN_POINT ( 'NONE',  ( -25.15625982127824400, 1.053316850513906111, -205.6460296093184184 ) ) ;
#8083 = CARTESIAN_POINT ( 'NONE',  ( 16.50094977371536231, 8.749999999999998224, -91.72275351520976017 ) ) ;
#8084 = APPROVAL_ROLE ( '' ) ;
#8085 = DIRECTION ( 'NONE',  ( -0.000000000000000000, 1.000000000000000000, -0.000000000000000000 ) ) ;
#8086 = CARTESIAN_POINT ( 'NONE',  ( 0.3766621274091715987, 0.5000000000000000000, 0.1491815183709511716 ) ) ;
#8087 = ORIENTED_EDGE ( 'NONE', *, *, #1589, .F. ) ;
#8088 = CARTESIAN_POINT ( 'NONE',  ( 3.249999999999998224, 7.187500000000000888, -4.846194077712561388 ) ) ;
#8089 = CARTESIAN_POINT ( 'NONE',  ( 10.28321301342407601, 14.39503880988861262, -106.6749965504387916 ) ) ;
#8090 = EDGE_CURVE ( 'NONE', #788, #9763, #7812, .T. ) ;
#8091 = CARTESIAN_POINT ( 'NONE',  ( 3.749999999999999556, 8.250000000000000000, -3.500000000000000444 ) ) ;
#8092 = EDGE_CURVE ( 'NONE', #14091, #3511, #374, .T. ) ;
#8093 = CARTESIAN_POINT ( 'NONE',  ( 3.749999999999999556, 14.81250000000000178, -1.946699141100892261 ) ) ;
#8094 = EDGE_CURVE ( 'NONE', #8895, #7450, #6072, .T. ) ;
#8095 = CARTESIAN_POINT ( 'NONE',  ( -64.45835881414798507, 14.99074302885292198, -184.2213710543591958 ) ) ;
#8096 = CARTESIAN_POINT ( 'NONE',  ( 0.4151132296555069545, 3.270056657667109956, -138.3403225835776311 ) ) ;
#8097 = CARTESIAN_POINT ( 'NONE',  ( -2.651650429449553314, 12.87500000000000000, -6.151650429449552426 ) ) ;
#8098 = DIRECTION ( 'NONE',  ( 0.000000000000000000, 0.000000000000000000, 1.000000000000000000 ) ) ;
#8099 = DATE_TIME_ROLE ( 'classification_date' ) ;
#8100 = CARTESIAN_POINT ( 'NONE',  ( 27.03835354040193195, 15.00000000000000000, -138.2189567750509980 ) ) ;
#8101 = ORIENTED_EDGE ( 'NONE', *, *, #552, .F. ) ;
#8102 = CARTESIAN_POINT ( 'NONE',  ( 8.117806577086446040, 2.126742365985535343, 4.858884805342907676 ) ) ;
#8103 = CARTESIAN_POINT ( 'NONE',  ( 1.346194077712558279, 2.562500000000000444, -6.750000000000000000 ) ) ;
#8104 = CARTESIAN_POINT ( 'NONE',  ( -66.89175632424894502, 14.99999999999999822, -193.0526493258840048 ) ) ;
#8105 = CARTESIAN_POINT ( 'NONE',  ( 3.249999999999999556, 1.250000000000000222, -3.500000000000000000 ) ) ;
#8106 = ORIENTED_EDGE ( 'NONE', *, *, #4054, .F. ) ;
#8107 = DIRECTION ( 'NONE',  ( 0.000000000000000000, 0.000000000000000000, -1.000000000000000000 ) ) ;
#8108 = LINE ( 'NONE', #3399, #11446 ) ;
#8109 = CARTESIAN_POINT ( 'NONE',  ( 6.154006371964378275, 12.51839902998314003, 4.611585984674669625 ) ) ;
#8110 = CARTESIAN_POINT ( 'NONE',  ( -0.06526978517750199604, -1.215333660157913752E-12, -101.7940732946817235 ) ) ;
#8111 = CARTESIAN_POINT ( 'NONE',  ( 3.249999999999999556, 12.25000000000000000, -3.500000000000000000 ) ) ;
#8112 = DIRECTION ( 'NONE',  ( 0.000000000000000000, -1.000000000000000000, 0.000000000000000000 ) ) ;
#8113 = CARTESIAN_POINT ( 'NONE',  ( -1.553300858899107073, 1.937500000000000222, -7.249999999999999112 ) ) ;
#8114 = CARTESIAN_POINT ( 'NONE',  ( 0.4616602863826355096, 0.000000000000000000, -0.1920150514337515824 ) ) ;
#8115 = CC_DESIGN_PERSON_AND_ORGANIZATION_ASSIGNMENT ( #2539, #13128, ( #10666 ) ) ;
#8116 = CARTESIAN_POINT ( 'NONE',  ( -8.886921396801785278, 10.34135959593272780, -105.5168766094550250 ) ) ;
#8117 = CARTESIAN_POINT ( 'NONE',  ( 25.66515063164039745, 2.145468714964426038, -137.2655343200625282 ) ) ;
#8118 = CARTESIAN_POINT ( 'NONE',  ( 3.698847099818734829, 12.64700925907840023, 4.332249626577416635 ) ) ;
#8119 = CARTESIAN_POINT ( 'NONE',  ( -3.249999999999999556, 14.25000000000000000, -3.499999999999999556 ) ) ;
#8120 = LINE ( 'NONE', #4503, #4949 ) ;
#8121 = CARTESIAN_POINT ( 'NONE',  ( -2.729969426660547871, 9.999999999999998224, -110.6850855677400602 ) ) ;
#8122 = ORIENTED_EDGE ( 'NONE', *, *, #14442, .T. ) ;
#8123 = VERTEX_POINT ( 'NONE', #5792 ) ;
#8124 = CARTESIAN_POINT ( 'NONE',  ( -5.763889103029394612, 4.000000000000000888, -181.7491934423408964 ) ) ;
#8125 = CARTESIAN_POINT ( 'NONE',  ( -1.553300858899107295, 3.437500000000000000, -7.250000000000000000 ) ) ;
#8126 = CARTESIAN_POINT ( 'NONE',  ( 2.651650429449552870, 4.125000000000000000, -6.151650429449553314 ) ) ;
#8127 = CARTESIAN_POINT ( 'NONE',  ( -7.534724830497282255, 2.500000000000000444, -106.8248685501097839 ) ) ;
#8128 = ORIENTED_EDGE ( 'NONE', *, *, #7622, .F. ) ;
#8129 = B_SPLINE_CURVE_WITH_KNOTS ( 'NONE', 3,
 ( #10396, #2055, #15131, #823 ),
 .UNSPECIFIED., .F., .F.,
 ( 4, 4 ),
 ( 2.110397319742239368E-07, 0.0001887751033478067336 ),
 .UNSPECIFIED. ) ;
#8130 =( BOUNDED_CURVE ( )  B_SPLINE_CURVE ( 3, ( #6813, #7264, #2563, #5109 ),
 .UNSPECIFIED., .F., .T. ) 
 B_SPLINE_CURVE_WITH_KNOTS ( ( 4, 4 ),
 ( 0.8013173358133321988, 1.595733058832763396 ),
 .UNSPECIFIED. ) 
 CURVE ( )  GEOMETRIC_REPRESENTATION_ITEM ( )  RATIONAL_B_SPLINE_CURVE ( ( 1.000000000000000000, 0.9480964748145740417, 0.9480964748145740417, 1.000000000000000000 ) ) 
 REPRESENTATION_ITEM ( '' )  );
#8131 = CARTESIAN_POINT ( 'NONE',  ( -1.346194077712559389, 13.06250000000000000, -0.2500000000000002220 ) ) ;
#8132 = CARTESIAN_POINT ( 'NONE',  ( -54.45540687913352684, 15.00000000000000000, -149.0501727868689557 ) ) ;
#8133 = LOCAL_TIME ( 12, 28, 20.00000000000000000, #7301 ) ;
#8134 = CARTESIAN_POINT ( 'NONE',  ( -8.117864242877150360, 12.74145370066594118, -105.1028050937847098 ) ) ;
#8135 = CARTESIAN_POINT ( 'NONE',  ( 3.249999999999999112, 2.812500000000000000, -2.153805922287439945 ) ) ;
#8136 = CARTESIAN_POINT ( 'NONE',  ( -2.810094634146505399, 7.379999999999995453, -48.88660647235757040 ) ) ;
#8137 = DIRECTION ( 'NONE',  ( -0.5425857474536051051, -0.8090169943749466741, 0.2260358588205426955 ) ) ;
#8138 = EDGE_CURVE ( 'NONE', #2052, #9239, #13652, .T. ) ;
#8139 = ORIENTED_EDGE ( 'NONE', *, *, #2194, .T. ) ;
#8140 = DIRECTION ( 'NONE',  ( -0.9997619372588931741, 0.000000000000000000, -0.02181900108494707127 ) ) ;
#8141 = CARTESIAN_POINT ( 'NONE',  ( 3.249999999999999556, 11.75000000000000000, -3.500000000000000000 ) ) ;
#8142 = ORIENTED_EDGE ( 'NONE', *, *, #5448, .F. ) ;
#8143 = ORIENTED_EDGE ( 'NONE', *, *, #1488, .T. ) ;
#8144 = CARTESIAN_POINT ( 'NONE',  ( 3.749999999999999556, 9.249999999999998224, -3.500000000000000444 ) ) ;
#8145 = CARTESIAN_POINT ( 'NONE',  ( -5.542419796536699472, 2.331468351712828340E-16, 11.20594165676177134 ) ) ;
#8146 = CARTESIAN_POINT ( 'NONE',  ( 3.749999999999999112, 6.187500000000001776, -5.053300858899108405 ) ) ;
#8147 = CARTESIAN_POINT ( 'NONE',  ( 2.298097038856279362, 5.375000000000000888, -1.201902961143720860 ) ) ;
#8148 = ORIENTED_EDGE ( 'NONE', *, *, #4578, .F. ) ;
#8149 = SECURITY_CLASSIFICATION ( '', '', #12865 ) ;
#8150 = CARTESIAN_POINT ( 'NONE',  ( -2.027137927702660214, 14.99999999999674927, -107.0032022125440818 ) ) ;
#8151 = CARTESIAN_POINT ( 'NONE',  ( -1.346194077712559389, 1.437500000000000000, -6.749999999999999112 ) ) ;
#8152 = CIRCLE ( 'NONE', #10132, 1.000000000000000888 ) ;
#8153 = AXIS2_PLACEMENT_3D ( 'NONE', #6159, #12032, #14216 ) ;
#8154 = CARTESIAN_POINT ( 'NONE',  ( -2.651650429449552870, 4.125000000000000000, -0.8483495705504462414 ) ) ;
#8155 = CARTESIAN_POINT ( 'NONE',  ( -24.98891949655539335, 1.707693810982847449, -206.9370818847572480 ) ) ;
#8156 = FACE_OUTER_BOUND ( 'NONE', #4979, .T. ) ;
#8157 = CARTESIAN_POINT ( 'NONE',  ( 4.492499072540838689, 0.000000000000000000, -2.611025101989581820 ) ) ;
#8158 = COORDINATED_UNIVERSAL_TIME_OFFSET ( 0, 0, .AHEAD. ) ;
#8159 = AXIS2_PLACEMENT_3D ( 'NONE', #14925, #5473, #4322 ) ;
#8160 = CARTESIAN_POINT ( 'NONE',  ( 2.220649286760296270, 2.192442743657398108, -1.000000000000001776 ) ) ;
#8161 = VECTOR ( 'NONE', #4198, 1000.000000000000000 ) ;
#8162 = ORIENTED_EDGE ( 'NONE', *, *, #14507, .T. ) ;
#8163 = EDGE_CURVE ( 'NONE', #14341, #6985, #5291, .T. ) ;
#8164 = CARTESIAN_POINT ( 'NONE',  ( -2.298097038856279362, 5.875000000000000888, -5.798097038856278473 ) ) ;
#8165 = CARTESIAN_POINT ( 'NONE',  ( -2.573490212646732278, 5.321094445766561876, -29.14997122992682321 ) ) ;
#8166 = VECTOR ( 'NONE', #10065, 1000.000000000000227 ) ;
#8167 = CARTESIAN_POINT ( 'NONE',  ( 1.553300858899109071, 8.437500000000000000, 0.2499999999999989175 ) ) ;
#8168 = CARTESIAN_POINT ( 'NONE',  ( -3.750000000000000000, 14.25000000000000000, -3.499999999999999112 ) ) ;
#8169 = CARTESIAN_POINT ( 'NONE',  ( -67.33687266635307367, 14.30069434016096430, -197.3216639972416715 ) ) ;
#8170 = CARTESIAN_POINT ( 'NONE',  ( -3.852746828226704334, -2.353283696435566785, -1.000000000000007772 ) ) ;
#8171 = CARTESIAN_POINT ( 'NONE',  ( -3.980102097228897738E-16, 1.084202172485504434E-16, -6.749999999999999112 ) ) ;
#8172 = CARTESIAN_POINT ( 'NONE',  ( -2.640059788692800335, 4.336808689942017736E-16, -114.1739744175401512 ) ) ;
#8173 = APPLICATION_CONTEXT ( 'configuration controlled 3d designs of mechanical parts and assemblies' ) ;
#8174 = COORDINATED_UNIVERSAL_TIME_OFFSET ( 0, 0, .AHEAD. ) ;
#8175 = PRODUCT_DEFINITION_SHAPE ( 'NONE', 'NONE',  #1046 ) ;
#8176 = CARTESIAN_POINT ( 'NONE',  ( 4.507463604512255806, 0.000000000000000000, 2.585105772303601945 ) ) ;
#8177 = ORIENTED_EDGE ( 'NONE', *, *, #10144, .F. ) ;
#8178 = ADVANCED_FACE ( 'NONE', ( #9117 ), #15155, .T. ) ;
#8179 = FACE_OUTER_BOUND ( 'NONE', #8694, .T. ) ;
#8180 = CARTESIAN_POINT ( 'NONE',  ( 0.000000000000000000, 4.000000000000000000, -0.2500000000000002220 ) ) ;
#8181 = EDGE_CURVE ( 'NONE', #3117, #2896, #4064, .T. ) ;
#8182 = CARTESIAN_POINT ( 'NONE',  ( -66.12309802906914058, 15.00000000000000000, -189.2880876859682644 ) ) ;
#8183 = EDGE_CURVE ( 'NONE', #8353, #7290, #620, .T. ) ;
#8184 = CARTESIAN_POINT ( 'NONE',  ( 2.298097038856279362, 8.375000000000000000, -1.201902961143720860 ) ) ;
#8185 = VERTEX_POINT ( 'NONE', #6480 ) ;
#8186 = CARTESIAN_POINT ( 'NONE',  ( -5.117107008561104564, 15.00000000000121858, -113.5915292474848854 ) ) ;
#8187 = CARTESIAN_POINT ( 'NONE',  ( -25.42339729827660832, 0.05949801409391321932, -200.8587921603110260 ) ) ;
#8188 = CARTESIAN_POINT ( 'NONE',  ( 1.346194077712560944, 0.9374999999999998890, -0.2500000000000010547 ) ) ;
#8189 = CARTESIAN_POINT ( 'NONE',  ( -2.298097038856279362, 10.87500000000000000, -5.798097038856278473 ) ) ;
#8190 = CARTESIAN_POINT ( 'NONE',  ( 5.000000000000000888, -1.083335593717820167E-31, -101.4583377608209531 ) ) ;
#8191 = CARTESIAN_POINT ( 'NONE',  ( 2.651650429449554203, 3.375000000000000444, -0.8483495705504471296 ) ) ;
#8192 = DIRECTION ( 'NONE',  ( 0.08794243244722427244, 0.000000000000000000, 0.9961255586397054218 ) ) ;
#8193 = DIRECTION ( 'NONE',  ( 0.000000000000000000, 0.000000000000000000, -1.000000000000000000 ) ) ;
#8194 = CARTESIAN_POINT ( 'NONE',  ( 25.77559445462507171, 2.285915182027296488, -137.2249222079316837 ) ) ;
#8195 = CARTESIAN_POINT ( 'NONE',  ( 0.9523100111875539842, 0.000000000000000000, 41.35525398876907133 ) ) ;
#8196 = CARTESIAN_POINT ( 'NONE',  ( -3.980102097228897245E-16, 11.50000000000000000, -6.749999999999999112 ) ) ;
#8197 = EDGE_CURVE ( 'NONE', #4481, #14016, #8208, .T. ) ;
#8198 = CARTESIAN_POINT ( 'NONE',  ( -4.751975593842658441, 14.96875058370196321, -103.3648980062157818 ) ) ;
#8199 = CARTESIAN_POINT ( 'NONE',  ( 9.939878312292631080, -7.806255641895631925E-15, -115.2320631035898657 ) ) ;
#8200 = ORIENTED_EDGE ( 'NONE', *, *, #11038, .T. ) ;
#8201 = ORIENTED_EDGE ( 'NONE', *, *, #6313, .F. ) ;
#8202 = CARTESIAN_POINT ( 'NONE',  ( -2.274567279739943881, 4.000000000000000000, -178.3664838788908469 ) ) ;
#8203 = CARTESIAN_POINT ( 'NONE',  ( -3.749999999999999556, 4.312500000000000888, -5.053300858899104853 ) ) ;
#8204 = CARTESIAN_POINT ( 'NONE',  ( 2.651650429449552870, 6.125000000000000000, -6.151650429449553314 ) ) ;
#8205 = CARTESIAN_POINT ( 'NONE',  ( 12.76858567064540217, 3.999999999993260502, -166.6103056774037441 ) ) ;
#8206 = VERTEX_POINT ( 'NONE', #12281 ) ;
#8207 = CARTESIAN_POINT ( 'NONE',  ( -5.492028030076452794, 0.1084047943351758581, -117.0085585369582475 ) ) ;
#8208 = CIRCLE ( 'NONE', #14147, 0.5000000000000004441 ) ;
#8209 = CARTESIAN_POINT ( 'NONE',  ( -3.980102097228897245E-16, 14.50000000000000000, -6.749999999999999112 ) ) ;
#8210 = CARTESIAN_POINT ( 'NONE',  ( -8.226857985479755442, 5.000000000000000000, -114.4011953629546099 ) ) ;
#8211 = CARTESIAN_POINT ( 'NONE',  ( 0.000000000000000000, 4.000000000000000000, 0.000000000000000000 ) ) ;
#8212 = SHAPE_REPRESENTATION_RELATIONSHIP ( 'NONE' , 'NONE' ,  #10790, #3532 ) ;
#8213 = CARTESIAN_POINT ( 'NONE',  ( -2.298097038856278918, 4.375000000000000000, -5.798097038856277585 ) ) ;
#8214 = CALENDAR_DATE ( 2026, 8, 10 ) ;
#8215 = FACE_OUTER_BOUND ( 'NONE', #12791, .T. ) ;
#8216 = CARTESIAN_POINT ( 'NONE',  ( 4.781732708726812220, 1.734723475976807094E-15, -121.0163674326759491 ) ) ;
#8217 = ORIENTED_EDGE ( 'NONE', *, *, #1681, .T. ) ;
#8218 = AXIS2_PLACEMENT_3D ( 'NONE', #13104, #12879, #8078 ) ;
#8219 = CARTESIAN_POINT ( 'NONE',  ( -5.317082570419811915, 15.00000000000000178, -126.7958533838912700 ) ) ;
#8220 = CARTESIAN_POINT ( 'NONE',  ( -3.249999999999999556, 14.31250000000000000, -4.846194077712557835 ) ) ;
#8221 = ORIENTED_EDGE ( 'NONE', *, *, #14256, .T. ) ;
#8222 = ORIENTED_EDGE ( 'NONE', *, *, #12623, .T. ) ;
#8223 = CARTESIAN_POINT ( 'NONE',  ( -5.599503270685788792, 2.331468351713656644E-16, 20.51657426689472885 ) ) ;
#8224 =( BOUNDED_SURFACE ( )  B_SPLINE_SURFACE ( 3, 2, ( 
 ( #11822, #2339, #5730 ),
 ( #11682, #7035, #12775 ),
 ( #6967, #2182, #11749 ),
 ( #8047, #15187, #1171 ) ),
 .UNSPECIFIED., .F., .F., .T. ) 
 B_SPLINE_SURFACE_WITH_KNOTS ( ( 4, 4 ),
 ( 3, 3 ),
 ( 4.712388980384689674, 4.907255421178648547 ),
 ( 0.000000000000000000, 1.000000000000000000 ),
 .UNSPECIFIED. ) 
 GEOMETRIC_REPRESENTATION_ITEM ( )  RATIONAL_B_SPLINE_SURFACE ( (
 ( 1.000000000000000000, 1.000000000000000000, 1.000000000000000000),
 ( 1.000000000000000000, 1.000004279931538065, 1.000000000000000000),
 ( 1.000000000000000000, 0.9936567599901997561, 1.000000000000000000),
 ( 1.000000000000000000, 0.9810773865977353569, 1.000000000000000000) ) ) 
 REPRESENTATION_ITEM ( '' )  SURFACE ( )  );
#8225 = CARTESIAN_POINT ( 'NONE',  ( -3.749999999999999556, 7.750000000000000888, -3.499999999999999112 ) ) ;
#8226 = CARTESIAN_POINT ( 'NONE',  ( 2.298097038856279362, 8.375000000000000000, -1.201902961143720860 ) ) ;
#8227 = VERTEX_POINT ( 'NONE', #8641 ) ;
#8228 = CARTESIAN_POINT ( 'NONE',  ( 3.559460973859760013, 15.00000000000000000, -107.0011611385528880 ) ) ;
#8229 = CARTESIAN_POINT ( 'NONE',  ( 0.000000000000000000, 3.000000000000000000, -0.2500000000000002220 ) ) ;
#8230 = CARTESIAN_POINT ( 'NONE',  ( -1.553300858899107295, 9.437500000000000000, -7.250000000000000000 ) ) ;
#8231 = AXIS2_PLACEMENT_3D ( 'NONE', #9655, #6172, #14386 ) ;
#8232 = CIRCLE ( 'NONE', #1078, 3.187847681061608540 ) ;
#8233 = CARTESIAN_POINT ( 'NONE',  ( -25.69889708084257762, 0.9650723257009210521, -205.4472600487935665 ) ) ;
#8234 = DIRECTION ( 'NONE',  ( 0.08794243244722427244, 0.000000000000000000, 0.9961255586397055328 ) ) ;
#8235 = CARTESIAN_POINT ( 'NONE',  ( -8.671560925439088408, -2.743867526398025447, -35.09585054340072219 ) ) ;
#8236 = CALENDAR_DATE ( 2026, 8, 10 ) ;
#8237 = CARTESIAN_POINT ( 'NONE',  ( -61.23004053993285112, 15.00000000000000355, -172.1684668291862863 ) ) ;
#8238 = ORIENTED_EDGE ( 'NONE', *, *, #7256, .F. ) ;
#8239 = AXIS2_PLACEMENT_3D ( 'NONE', #4421, #14615, #13369 ) ;
#8240 = CARTESIAN_POINT ( 'NONE',  ( -3.980102097228897738E-16, 8.999999999999998224, -6.749999999999999112 ) ) ;
#8241 = CARTESIAN_POINT ( 'NONE',  ( -7.194037649453649763, 1.020558061026469510, -45.55632290616381397 ) ) ;
#8242 = CARTESIAN_POINT ( 'NONE',  ( 3.749999999999999112, 12.31250000000000178, -1.946699141100893149 ) ) ;
#8243 = CARTESIAN_POINT ( 'NONE',  ( -5.794432043291358525, 13.40945642053105225, -125.0404107129116085 ) ) ;
#8244 = ADVANCED_FACE ( 'NONE', ( #14624 ), #5252, .T. ) ;
#8245 = CARTESIAN_POINT ( 'NONE',  ( -67.48102662054394330, 13.98401442981596077, -198.9466073721665396 ) ) ;
#8246 = CARTESIAN_POINT ( 'NONE',  ( -0.04436259091852395170, 5.000000000000007105, -136.3368594361672876 ) ) ;
#8247 = CARTESIAN_POINT ( 'NONE',  ( 3.750000000000000000, 13.31250000000000178, -1.946699141100892705 ) ) ;
#8248 = TOROIDAL_SURFACE ( 'NONE', #3074, 5.000000000000001776, 5.000000000000000000 ) ;
#8249 = CARTESIAN_POINT ( 'NONE',  ( 9.161239424535876807, 0.8923617020344253303, -105.7786917259425508 ) ) ;
#8250 = PERSON_AND_ORGANIZATION ( #3176, #3020 ) ;
#8251 = CARTESIAN_POINT ( 'NONE',  ( -3.249999999999999556, 14.18750000000000000, -2.153805922287440833 ) ) ;
#8252 = DIRECTION ( 'NONE',  ( 0.000000000000000000, 0.000000000000000000, -1.000000000000000000 ) ) ;
#8253 = EDGE_LOOP ( 'NONE', ( #12826, #10823, #8222, #6990 ) ) ;
#8254 = CARTESIAN_POINT ( 'NONE',  ( 6.108231453664635602, 4.487270727616577304, 5.259165607916492569 ) ) ;
#8255 = CARTESIAN_POINT ( 'NONE',  ( 1.346194077712560944, 1.937500000000000000, -0.2500000000000011102 ) ) ;
#8256 = CARTESIAN_POINT ( 'NONE',  ( -59.62538729150122663, 15.00000000000000000, -184.0486941882522842 ) ) ;
#8257 = CARTESIAN_POINT ( 'NONE',  ( 3.249999999999999556, 5.250000000000000000, -3.500000000000000000 ) ) ;
#8258 = ORIENTED_EDGE ( 'NONE', *, *, #2307, .F. ) ;
#8259 = CARTESIAN_POINT ( 'NONE',  ( -6.422940335267006695, 14.99999999999267963, -108.3014594333919973 ) ) ;
#8260 = CARTESIAN_POINT ( 'NONE',  ( -25.82983890416511841, 9.999999999999998224, -152.2527639562405000 ) ) ;
#8261 = DIRECTION ( 'NONE',  ( 0.000000000000000000, 0.000000000000000000, -1.000000000000000000 ) ) ;
#8262 = CARTESIAN_POINT ( 'NONE',  ( 0.000000000000000000, 0.000000000000000000, -0.2500000000000002220 ) ) ;
#8263 = CARTESIAN_POINT ( 'NONE',  ( -1.346194077712558945, 12.56250000000000355, -0.2500000000000002220 ) ) ;
#8264 = CARTESIAN_POINT ( 'NONE',  ( -3.750000000000000000, 7.187500000000000000, -1.946699141100892927 ) ) ;
#8265 = LINE ( 'NONE', #10441, #3227 ) ;
#8266 = CARTESIAN_POINT ( 'NONE',  ( -3.750000000000000000, 3.687500000000000444, -1.946699141100893149 ) ) ;
#8267 = CARTESIAN_POINT ( 'NONE',  ( 1.893911505664648054, 15.00000000000000000, -1.663006917529762152 ) ) ;
#8268 = EDGE_CURVE ( 'NONE', #9864, #11348, #14905, .T. ) ;
#8269 = DIRECTION ( 'NONE',  ( -0.000000000000000000, -1.000000000000000000, -0.000000000000000000 ) ) ;
#8270 = DIRECTION ( 'NONE',  ( -0.002879925520664897674, 0.000000000000000000, -0.9999958530058988826 ) ) ;
#8271 = CARTESIAN_POINT ( 'NONE',  ( 3.230086961373112242, 9.999999999999998224, 5.208283729180105404 ) ) ;
#8272 = CARTESIAN_POINT ( 'NONE',  ( 2.298097038856279362, 10.87500000000000178, -1.201902961143720860 ) ) ;
#8273 = CARTESIAN_POINT ( 'NONE',  ( -5.714611007916760244, 14.75484434184808613, -103.6239156122758942 ) ) ;
#8274 = CARTESIAN_POINT ( 'NONE',  ( -3.691420245339818607, 9.999999999999998224, -128.6724311331325339 ) ) ;
#8275 = EDGE_LOOP ( 'NONE', ( #3745, #4878 ) ) ;
#8276 = EDGE_LOOP ( 'NONE', ( #3160, #14818, #12587, #486 ) ) ;
#8277 = CARTESIAN_POINT ( 'NONE',  ( -5.257674075046501194, 4.336808689942017736E-16, -105.6497928282025214 ) ) ;
#8278 = CARTESIAN_POINT ( 'NONE',  ( 8.246457104576641939, 8.673617379884035472E-16, -163.7205653903581037 ) ) ;
#8279 = CARTESIAN_POINT ( 'NONE',  ( 2.651650429449553759, 5.875000000000000000, -0.8483495705504471296 ) ) ;
#8280 = CARTESIAN_POINT ( 'NONE',  ( 1.553300858899109071, 5.437500000000000888, 0.2499999999999989175 ) ) ;
#8281 = CARTESIAN_POINT ( 'NONE',  ( 3.130150272509794274, 1.749999999999379829, 2.913007886993950191 ) ) ;
#8282 = ORIENTED_EDGE ( 'NONE', *, *, #5701, .T. ) ;
#8283 = CARTESIAN_POINT ( 'NONE',  ( 2.298097038856279362, 14.87500000000000178, -1.201902961143720860 ) ) ;
#8284 = B_SPLINE_CURVE_WITH_KNOTS ( 'NONE', 3,
 ( #10880, #10572, #3689, #11801 ),
 .UNSPECIFIED., .F., .F.,
 ( 4, 4 ),
 ( 0.000000000000000000, 0.0004294366880267255987 ),
 .UNSPECIFIED. ) ;
#8285 = CARTESIAN_POINT ( 'NONE',  ( 0.2499999999999999445, 4.500000000000000888, 1.500000000000000222 ) ) ;
#8286 = EDGE_CURVE ( 'NONE', #13498, #10617, #1815, .T. ) ;
#8287 = CARTESIAN_POINT ( 'NONE',  ( 6.117677467307099270, 8.673617379884035472E-16, -123.7586964171227066 ) ) ;
#8288 = CARTESIAN_POINT ( 'NONE',  ( -6.938893903907228378E-15, 4.781808091008227457, -138.5079647995998471 ) ) ;
#8289 = CARTESIAN_POINT ( 'NONE',  ( 3.249999999999999112, 4.812500000000000888, -2.153805922287439945 ) ) ;
#8290 = B_SPLINE_CURVE_WITH_KNOTS ( 'NONE', 3,
 ( #14890, #4287, #13867, #581, #11239, #10079, #14741, #14814, #3119, #4360, #9069, #13790, #7039, #2186, #2411, #10597, #1176, #13946, #5957, #9363, #12853, #5877, #10453, #10679 ),
 .UNSPECIFIED., .F., .F.,
 ( 4, 2, 2, 2, 2, 2, 2, 2, 2, 2, 2, 4 ),
 ( 1.734723475976807094E-18, 0.002712057318076011199, 0.005424114636152054490, 0.008136171954228096914, 0.01084822927230414021, 0.01220425793134216272, 0.01356028659038018523, 0.01491631524941820601, 0.01627234390845622852, 0.01898440122653227008, 0.02034042988557029086, 0.02169645854460831164 ),
 .UNSPECIFIED. ) ;
#8291 = CARTESIAN_POINT ( 'NONE',  ( -1.500000000000000000, 4.500000000000000888, 0.2500000000000002220 ) ) ;
#8292 = CARTESIAN_POINT ( 'NONE',  ( 3.843629782151245955, 8.673617379884035472E-16, -118.2118429041878898 ) ) ;
#8293 = VERTEX_POINT ( 'NONE', #389 ) ;
#8294 = PLANE ( 'NONE',  #9997 ) ;
#8295 = DIRECTION ( 'NONE',  ( 0.000000000000000000, 0.000000000000000000, -1.000000000000000000 ) ) ;
#8296 = VERTEX_POINT ( 'NONE', #8563 ) ;
#8297 = VERTEX_POINT ( 'NONE', #4102 ) ;
#8298 = CARTESIAN_POINT ( 'NONE',  ( 16.50094977371536231, 8.749999999999998224, -91.72275351520976017 ) ) ;
#8299 = CARTESIAN_POINT ( 'NONE',  ( -1.553300858899107073, 5.937500000000002665, -7.249999999999999112 ) ) ;
#8300 = CARTESIAN_POINT ( 'NONE',  ( -3.249999999999999556, 4.750000000000000888, -3.500000000000000000 ) ) ;
#8301 = ORIENTED_EDGE ( 'NONE', *, *, #5832, .T. ) ;
#8302 = CARTESIAN_POINT ( 'NONE',  ( 3.743303269469635097, 14.99999999999999822, -106.5640776127148399 ) ) ;
#8303 = CARTESIAN_POINT ( 'NONE',  ( -1.346194077712559389, 3.437500000000000000, -6.749999999999999112 ) ) ;
#8304 = PRODUCT ( 'Blade_Predeterminado', 'Blade_Predeterminado', '', ( #3616 ) ) ;
#8305 = CARTESIAN_POINT ( 'NONE',  ( -5.247127501425628893, 2.500000000000000444, -111.6612542950777254 ) ) ;
#8306 = CARTESIAN_POINT ( 'NONE',  ( -3.234594381879578151, 7.379999999999995453, -42.32384790875221370 ) ) ;
#8307 = CARTESIAN_POINT ( 'NONE',  ( 8.283327938524582379, 15.00000000000000000, -122.5135224137794978 ) ) ;
#8308 = PERSON_AND_ORGANIZATION ( #3176, #3020 ) ;
#8309 = CARTESIAN_POINT ( 'NONE',  ( 3.009961423602985242, 0.9636447990543508535, -1.000000000000001332 ) ) ;
#8310 =( BOUNDED_CURVE ( )  B_SPLINE_CURVE ( 2, ( #6468, #10103, #12272, #11184, #4240, #1842, #2853, #3071, #10029, #758, #7553, #7705, #4164, #11335, #7785, #13366, #8866, #5389, #4011, #2922, #12192, #14840, #12498, #1610, #14612, #5468, #6549, #11261, #8713, #8944, #684, #13672, #5163, #1915, #6628, #11037, #1680, #7624, #6393, #11105, #9951, #14689, #4091, #8794, #14920, #836, #4316, #3142, #9020, #5541, #13745, #7856, #12574, #1988, #6705, #11417, #1547, #14304, #2397, #7408, #9507, #14231, #7333, #6260, #10741, #10977, #156, #7093, #10811, #12993, #7257, #5103, #12131, #10665, #4794, #9658, #9745, #11814, #1234, #227, #2631, #3633, #12044, #5026, #4865, #13228, #14389, #11891, #14473, #394, #8495, #1314, #8413, #10896, #9577, #6020, #14158, #3788, #1393, #11973, #8335, #13060, #6096, #3870, #7171, #4943, #8571, #1465, #2475, #13304, #6177, #3559, #3705, #312, #2706, #8264, #5942, #82, #13145, #2555, #9893, #6338, #469, #5401, #3083, #7491, #5181, #11345, #10042, #14779, #14629, #10115, #3015, #8880, #11052, #7797, #14857, #13686, #12210, #13537, #1625, #774, #1857, #4176, #4026, #11202, #8731, #13613, #7721, #7640, #4106, #12507, #8955, #12285, #6638, #12435, #8807, #6562, #13464, #11275, #9818, #1926, #2867, #14550, #696, #8649, #7566, #3945, #4254, #13383, #624, #11127, #2789, #14706, #1695, #2936, #6407, #543, #5256, #9966, #12359, #1776, #6485, #5330, #15232, #14999, #10198, #14932, #4552, #11723, #920, #989, #3151, #12818, #4472, #5776, #4328, #9335, #4624, #4396, #9031, #15075, #11572, #12584, #2224, #3456, #5480, #13756, #11651, #7865, #9260, #10499, #13985, #14057, #13826, #6860, #2002, #10420, #10266, #11505, #5551, #6713, #11426, #6934, #9182, #9104, #12745, #3230, #8168, #12896, #12663, #2306, #848, #3311, #7943, #5700, #13913, #8093, #5621, #2079, #6791 ),
 .UNSPECIFIED., .F., .F. ) 
 B_SPLINE_CURVE_WITH_KNOTS ( ( 3, 2, 2, 2, 2, 2, 2, 2, 2, 2, 2, 2, 2, 2, 2, 2, 2, 2, 2, 2, 2, 2, 2, 2, 2, 2, 2, 2, 2, 2, 2, 2, 2, 2, 2, 2, 2, 2, 2, 2, 2, 2, 2, 2, 2, 2, 2, 2, 2, 2, 2, 2, 2, 2, 2, 2, 2, 2, 2, 2, 2, 2, 2, 2, 2, 2, 2, 2, 2, 2, 2, 2, 2, 2, 2, 2, 2, 2, 2, 2, 2, 2, 2, 2, 2, 2, 2, 2, 2, 2, 2, 2, 2, 2, 2, 2, 2, 2, 2, 2, 2, 2, 2, 2, 2, 2, 2, 2, 2, 2, 2, 2, 2, 2, 2, 2, 2, 2, 2, 2, 3 ),
 ( 0.000000000000000000, 0.008333333333333333218, 0.01666666666666666644, 0.02500000000000000139, 0.03333333333333333287, 0.04166666666666666435, 0.05000000000000000278, 0.05833333333333333426, 0.06666666666666666574, 0.07499999999999999722, 0.08333333333333332871, 0.09166666666666666019, 0.1000000000000000056, 0.1083333333333333370, 0.1166666666666666685, 0.1250000000000000000, 0.1333333333333333315, 0.1416666666666666630, 0.1499999999999999944, 0.1583333333333333259, 0.1666666666666666574, 0.1749999999999999889, 0.1833333333333333204, 0.1916666666666666519, 0.2000000000000000111, 0.2083333333333333426, 0.2166666666666666741, 0.2250000000000000056, 0.2333333333333333370, 0.2416666666666666685, 0.2500000000000000000, 0.2583333333333333037, 0.2666666666666666630, 0.2750000000000000222, 0.2833333333333333259, 0.2916666666666666852, 0.2999999999999999889, 0.3083333333333333481, 0.3166666666666666519, 0.3250000000000000111, 0.3333333333333333148, 0.3416666666666666741, 0.3499999999999999778, 0.3583333333333333370, 0.3666666666666666408, 0.3750000000000000000, 0.3833333333333333037, 0.3916666666666666630, 0.4000000000000000222, 0.4083333333333333259, 0.4166666666666666852, 0.4249999999999999889, 0.4333333333333333481, 0.4416666666666666519, 0.4500000000000000111, 0.4583333333333333148, 0.4666666666666666741, 0.4749999999999999778, 0.4833333333333333370, 0.4916666666666666408, 0.5000000000000000000, 0.5083333333333333037, 0.5166666666666666075, 0.5250000000000000222, 0.5333333333333333259, 0.5416666666666666297, 0.5500000000000000444, 0.5583333333333333481, 0.5666666666666666519, 0.5749999999999999556, 0.5833333333333333703, 0.5916666666666666741, 0.5999999999999999778, 0.6083333333333332815, 0.6166666666666666963, 0.6250000000000000000, 0.6333333333333333037, 0.6416666666666666075, 0.6500000000000000222, 0.6583333333333333259, 0.6666666666666666297, 0.6750000000000000444, 0.6833333333333333481, 0.6916666666666666519, 0.6999999999999999556, 0.7083333333333333703, 0.7166666666666666741, 0.7249999999999999778, 0.7333333333333332815, 0.7416666666666666963, 0.7500000000000000000, 0.7583333333333333037, 0.7666666666666666075, 0.7750000000000000222, 0.7833333333333333259, 0.7916666666666666297, 0.8000000000000000444, 0.8083333333333333481, 0.8166666666666666519, 0.8249999999999999556, 0.8333333333333333703, 0.8416666666666666741, 0.8499999999999999778, 0.8583333333333332815, 0.8666666666666666963, 0.8750000000000000000, 0.8833333333333333037, 0.8916666666666666075, 0.9000000000000000222, 0.9083333333333333259, 0.9166666666666666297, 0.9249999999999999334, 0.9333333333333333481, 0.9416666666666666519, 0.9499999999999999556, 0.9583333333333333703, 0.9666666666666666741, 0.9749999999999999778, 0.9833333333333332815, 0.9916666666666666963, 1.000000000000000000 ),
 .UNSPECIFIED. ) 
 CURVE ( )  GEOMETRIC_REPRESENTATION_ITEM ( )  RATIONAL_B_SPLINE_CURVE ( ( 1.000000000000000000, 0.9238795325112867385, 1.000000000000000000, 0.9238795325112867385, 1.000000000000000000, 0.9238795325112867385, 1.000000000000000000, 0.9238795325112867385, 1.000000000000000000, 0.9238795325112867385, 1.000000000000000000, 0.9238795325112867385, 1.000000000000000000, 0.9238795325112867385, 1.000000000000000000, 0.9238795325112867385, 1.000000000000000000, 0.9238795325112867385, 1.000000000000000000, 0.9238795325112867385, 1.000000000000000000, 0.9238795325112867385, 1.000000000000000000, 0.9238795325112867385, 1.000000000000000000, 0.9238795325112867385, 1.000000000000000000, 0.9238795325112867385, 1.000000000000000000, 0.9238795325112867385, 1.000000000000000000, 0.9238795325112867385, 1.000000000000000000, 0.9238795325112867385, 1.000000000000000000, 0.9238795325112867385, 1.000000000000000000, 0.9238795325112867385, 1.000000000000000000, 0.9238795325112867385, 1.000000000000000000, 0.9238795325112867385, 1.000000000000000000, 0.9238795325112867385, 1.000000000000000000, 0.9238795325112867385, 1.000000000000000000, 0.9238795325112867385, 1.000000000000000000, 0.9238795325112867385, 1.000000000000000000, 0.9238795325112867385, 1.000000000000000000, 0.9238795325112867385, 1.000000000000000000, 0.9238795325112867385, 1.000000000000000000, 0.9238795325112867385, 1.000000000000000000, 0.9238795325112867385, 1.000000000000000000, 0.9238795325112867385, 1.000000000000000000, 0.9238795325112867385, 1.000000000000000000, 0.9238795325112867385, 1.000000000000000000, 0.9238795325112867385, 1.000000000000000000, 0.9238795325112867385, 1.000000000000000000, 0.9238795325112867385, 1.000000000000000000, 0.9238795325112867385, 1.000000000000000000, 0.9238795325112867385, 1.000000000000000000, 0.9238795325112867385, 1.000000000000000000, 0.9238795325112867385, 1.000000000000000000, 0.9238795325112867385, 1.000000000000000000, 0.9238795325112867385, 1.000000000000000000, 0.9238795325112867385, 1.000000000000000000, 0.9238795325112867385, 1.000000000000000000, 0.9238795325112867385, 1.000000000000000000, 0.9238795325112867385, 1.000000000000000000, 0.9238795325112867385, 1.000000000000000000, 0.9238795325112867385, 1.000000000000000000, 0.9238795325112867385, 1.000000000000000000, 0.9238795325112867385, 1.000000000000000000, 0.9238795325112867385, 1.000000000000000000, 0.9238795325112867385, 1.000000000000000000, 0.9238795325112867385, 1.000000000000000000, 0.9238795325112867385, 1.000000000000000000, 0.9238795325112867385, 1.000000000000000000, 0.9238795325112867385, 1.000000000000000000, 0.9238795325112867385, 1.000000000000000000, 0.9238795325112867385, 1.000000000000000000, 0.9238795325112867385, 1.000000000000000000, 0.9238795325112867385, 1.000000000000000000, 0.9238795325112867385, 1.000000000000000000, 0.9238795325112867385, 1.000000000000000000, 0.9238795325112867385, 1.000000000000000000, 0.9238795325112867385, 1.000000000000000000, 0.9238795325112867385, 1.000000000000000000, 0.9238795325112867385, 1.000000000000000000, 0.9238795325112867385, 1.000000000000000000, 0.9238795325112867385, 1.000000000000000000, 0.9238795325112867385, 1.000000000000000000, 0.9238795325112867385, 1.000000000000000000, 0.9238795325112867385, 1.000000000000000000, 0.9238795325112867385, 1.000000000000000000, 0.9238795325112867385, 1.000000000000000000, 0.9238795325112867385, 1.000000000000000000, 0.9238795325112867385, 1.000000000000000000, 0.9238795325112867385, 1.000000000000000000, 0.9238795325112867385, 1.000000000000000000, 0.9238795325112867385, 1.000000000000000000, 0.9238795325112867385, 1.000000000000000000, 0.9238795325112867385, 1.000000000000000000, 0.9238795325112867385, 1.000000000000000000, 0.9238795325112867385, 1.000000000000000000, 0.9238795325112867385, 1.000000000000000000, 0.9238795325112867385, 1.000000000000000000, 0.9238795325112867385, 1.000000000000000000, 0.9238795325112867385, 1.000000000000000000, 0.9238795325112867385, 1.000000000000000000, 0.9238795325112867385, 1.000000000000000000, 0.9238795325112867385, 1.000000000000000000, 0.9238795325112867385, 1.000000000000000000, 0.9238795325112867385, 1.000000000000000000, 0.9238795325112867385, 1.000000000000000000, 0.9238795325112867385, 1.000000000000000000, 0.9238795325112867385, 1.000000000000000000, 0.9238795325112867385, 1.000000000000000000, 0.9238795325112867385, 1.000000000000000000, 0.9238795325112867385, 1.000000000000000000, 0.9238795325112867385, 1.000000000000000000, 0.9238795325112867385, 1.000000000000000000, 0.9238795325112867385, 1.000000000000000000, 0.9238795325112867385, 1.000000000000000000, 0.9238795325112867385, 1.000000000000000000, 0.9238795325112867385, 1.000000000000000000, 0.9238795325112867385, 1.000000000000000000, 0.9238795325112867385, 1.000000000000000000, 0.9238795325112867385, 1.000000000000000000, 0.9238795325112867385, 1.000000000000000000, 0.9238795325112867385, 1.000000000000000000, 0.9238795325112867385, 1.000000000000000000, 0.9238795325112867385, 1.000000000000000000, 0.9238795325112867385, 1.000000000000000000, 0.9238795325112867385, 1.000000000000000000, 0.9238795325112867385, 1.000000000000000000, 0.9238795325112867385, 1.000000000000000000, 0.9238795325112867385, 1.000000000000000000, 0.9238795325112867385, 1.000000000000000000, 0.9238795325112867385, 1.000000000000000000, 0.9238795325112867385, 1.000000000000000000, 0.9238795325112867385, 1.000000000000000000, 0.9238795325112867385, 1.000000000000000000 ) ) 
 REPRESENTATION_ITEM ( '' )  );
#8311 = VECTOR ( 'NONE', #8689, 1000.000000000000000 ) ;
#8312 = ORIENTED_EDGE ( 'NONE', *, *, #15306, .T. ) ;
#8313 = CARTESIAN_POINT ( 'NONE',  ( 8.475206276408092876, 0.000000000000000000, -34.56909192082981974 ) ) ;
#8314 = CARTESIAN_POINT ( 'NONE',  ( 3.749999999999999112, 14.31250000000000355, -1.946699141100893149 ) ) ;
#8315 = CYLINDRICAL_SURFACE ( 'NONE', #2001, 3.500000000000003109 ) ;
#8316 = CARTESIAN_POINT ( 'NONE',  ( -63.81341264818736647, 12.59430211938071764, -202.1382658931505887 ) ) ;
#8317 = CARTESIAN_POINT ( 'NONE',  ( -3.542861251344865181, 5.000000000000010658, -131.3727830290921190 ) ) ;
#8318 = CARTESIAN_POINT ( 'NONE',  ( -3.249999999999999556, 1.750000000000000222, -3.500000000000000000 ) ) ;
#8319 = CARTESIAN_POINT ( 'NONE',  ( 10.97171279554003043, 8.773889247172311556, -44.61149169061435060 ) ) ;
#8320 = APPLICATION_PROTOCOL_DEFINITION ( 'international standard', 'config_control_design', 1994, #7479 ) ;
#8321 = DIRECTION ( 'NONE',  ( -0.000000000000000000, -1.000000000000000000, -0.000000000000000000 ) ) ;
#8322 = CARTESIAN_POINT ( 'NONE',  ( -16.02909037268676329, 1.021521734388686209E-15, -131.4942061907987068 ) ) ;
#8323 = ORIENTED_EDGE ( 'NONE', *, *, #10540, .T. ) ;
#8324 = CARTESIAN_POINT ( 'NONE',  ( 4.027501057062753631, 0.09548388211871727815, -1.357275530841774991 ) ) ;
#8325 = CARTESIAN_POINT ( 'NONE',  ( 1.346194077712558279, 3.562500000000000000, -6.750000000000000000 ) ) ;
#8326 = FACE_OUTER_BOUND ( 'NONE', #12002, .T. ) ;
#8327 = CARTESIAN_POINT ( 'NONE',  ( -3.980102097228897738E-16, 7.000000000000000000, -6.749999999999999112 ) ) ;
#8328 = ORIENTED_EDGE ( 'NONE', *, *, #10642, .T. ) ;
#8329 = CARTESIAN_POINT ( 'NONE',  ( -5.447453277264131088, 15.00000000000000178, -116.0587048211255166 ) ) ;
#8330 = UNCERTAINTY_MEASURE_WITH_UNIT (LENGTH_MEASURE( 1.000000000000000082E-05 ), #2275, 'distance_accuracy_value', 'NONE');
#8331 = CARTESIAN_POINT ( 'NONE',  ( 0.000000000000000000, 15.00000000000000000, 0.000000000000000000 ) ) ;
#8332 = CARTESIAN_POINT ( 'NONE',  ( 8.054779650714358752, 9.999999999999998224, -130.1950568140816813 ) ) ;
#8333 = FACE_OUTER_BOUND ( 'NONE', #13789, .T. ) ;
#8334 = CARTESIAN_POINT ( 'NONE',  ( 2.651650429449553314, 2.375000000000000000, -0.8483495705504476847 ) ) ;
#8335 = CARTESIAN_POINT ( 'NONE',  ( -3.750000000000000000, 6.250000000000000000, -3.499999999999999112 ) ) ;
#8336 = CARTESIAN_POINT ( 'NONE',  ( 17.33677725113053114, 5.000000000000000888, -156.7678757841025003 ) ) ;
#8337 = CARTESIAN_POINT ( 'NONE',  ( -4.592425496802573972E-16, 5.000000000000000000, -7.250000000000000000 ) ) ;
#8338 = CARTESIAN_POINT ( 'NONE',  ( 2.858579147729096714, 14.48245223601180953, 0.7576670880602638380 ) ) ;
#8339 = CARTESIAN_POINT ( 'NONE',  ( -3.805429041573433313, 11.11311992875805288, -44.52694620552966853 ) ) ;
#8340 = CARTESIAN_POINT ( 'NONE',  ( -8.429367341598160479, 0.9564791310987349471, -105.2145337967942282 ) ) ;
#8341 = CARTESIAN_POINT ( 'NONE',  ( -5.661351488087990269, 3.999999999999993783, -144.3936414932596506 ) ) ;
#8342 = CARTESIAN_POINT ( 'NONE',  ( -3.249999999999999556, 12.25000000000000000, -3.499999999999999556 ) ) ;
#8343 = CYLINDRICAL_SURFACE ( 'NONE', #4711, 14.80000000000025651 ) ;
#8344 = CARTESIAN_POINT ( 'NONE',  ( -63.35291325964459475, 11.28823943156841203, -203.2975719163582653 ) ) ;
#8345 = ORIENTED_EDGE ( 'NONE', *, *, #1644, .F. ) ;
#8346 = EDGE_CURVE ( 'NONE', #8297, #10459, #1770, .T. ) ;
#8347 = EDGE_LOOP ( 'NONE', ( #7656, #7104, #10321, #3546 ) ) ;
#8348 = CARTESIAN_POINT ( 'NONE',  ( -5.114912396505194359, 2.500000000000000444, -113.5322278711313260 ) ) ;
#8349 = CARTESIAN_POINT ( 'NONE',  ( 13.05679544828472238, 4.000000000000000000, -166.4200500252868551 ) ) ;
#8350 = CARTESIAN_POINT ( 'NONE',  ( -3.749999999999999556, 3.312500000000000000, -5.053300858899104853 ) ) ;
#8351 = CARTESIAN_POINT ( 'NONE',  ( 0.000000000000000000, 2.500000000000000000, 0.2499999999999998057 ) ) ;
#8352 = DIRECTION ( 'NONE',  ( 0.000000000000000000, 0.000000000000000000, -1.000000000000000000 ) ) ;
#8353 = VERTEX_POINT ( 'NONE', #8724 ) ;
#8354 = CARTESIAN_POINT ( 'NONE',  ( 3.249999999999998224, 3.312500000000000000, -2.153805922287439945 ) ) ;
#8355 = CARTESIAN_POINT ( 'NONE',  ( -63.69159315064205629, 9.999999999999998224, -164.7787203863022967 ) ) ;
#8356 = DIRECTION ( 'NONE',  ( 0.000000000000000000, 0.000000000000000000, 1.000000000000000000 ) ) ;
#8357 =( LENGTH_UNIT ( ) NAMED_UNIT ( * ) SI_UNIT ( .MILLI., .METRE. ) );
#8358 = CARTESIAN_POINT ( 'NONE',  ( 1.346194077712560944, 7.937500000000000888, -0.2500000000000010547 ) ) ;
#8359 = FACE_OUTER_BOUND ( 'NONE', #1671, .T. ) ;
#8360 = COORDINATED_UNIVERSAL_TIME_OFFSET ( 0, 0, .AHEAD. ) ;
#8361 = CARTESIAN_POINT ( 'NONE',  ( 1.500000000000000000, 5.000000000000000000, 0.2500000000000002220 ) ) ;
#8362 = CARTESIAN_POINT ( 'NONE',  ( 9.723706525289889768, -3.022969897739336727E-12, -119.8316069321379302 ) ) ;
#8363 = ORIENTED_EDGE ( 'NONE', *, *, #76, .T. ) ;
#8364 = CARTESIAN_POINT ( 'NONE',  ( -0.5514805362514287879, 14.99999999999999645, -109.6828893904346813 ) ) ;
#8365 = CARTESIAN_POINT ( 'NONE',  ( 2.298097038856279362, 14.87500000000000178, -1.201902961143720860 ) ) ;
#8366 = EDGE_LOOP ( 'NONE', ( #12796, #10770 ) ) ;
#8367 = ADVANCED_FACE ( 'NONE', ( #6255 ), #6402, .F. ) ;
#8368 = ORIENTED_EDGE ( 'NONE', *, *, #9798, .F. ) ;
#8369 = FACE_OUTER_BOUND ( 'NONE', #4002, .T. ) ;
#8370 = CARTESIAN_POINT ( 'NONE',  ( -3.750000000000000000, 5.687500000000000888, -1.946699141100893149 ) ) ;
#8371 = EDGE_CURVE ( 'NONE', #5472, #14341, #8650, .T. ) ;
#8372 = CARTESIAN_POINT ( 'NONE',  ( -3.249999999999999112, 11.68749999999999822, -2.153805922287440833 ) ) ;
#8374 = EDGE_CURVE ( 'NONE', #5152, #4454, #6931, .T. ) ;
#8373 = ORIENTED_EDGE ( 'NONE', *, *, #2304, .F. ) ;
#8375 = CARTESIAN_POINT ( 'NONE',  ( -3.294555838625194077, 14.99999999999918643, -108.9576586821702620 ) ) ;
#8376 = CARTESIAN_POINT ( 'NONE',  ( 0.000000000000000000, 7.000000000000000000, -0.2500000000000002220 ) ) ;
#8377 = SECURITY_CLASSIFICATION ( '', '', #14520 ) ;
#8378 = APPROVAL ( #2163, 'UNSPECIFIED' ) ;
#8379 = AXIS2_PLACEMENT_3D ( 'NONE', #15049, #14030, #11403 ) ;
#8380 = CARTESIAN_POINT ( 'NONE',  ( -24.60401395879240738, 4.143790226087491035, -208.9577473736382842 ) ) ;
#8381 = PLANE ( 'NONE',  #12883 ) ;
#8382 = VECTOR ( 'NONE', #6797, 1000.000000000000000 ) ;
#8383 = DATE_AND_TIME ( #10712, #2719 ) ;
#8384 = CARTESIAN_POINT ( 'NONE',  ( 3.128580254545037853, 0.4878928319773999656, -1.000000000000001110 ) ) ;
#8385 = LOCAL_TIME ( 12, 28, 20.00000000000000000, #6048 ) ;
#8386 = ORIENTED_EDGE ( 'NONE', *, *, #12239, .T. ) ;
#8387 = AXIS2_PLACEMENT_3D ( 'NONE', #7114, #8519, #10606 ) ;
#8388 = CC_DESIGN_PERSON_AND_ORGANIZATION_ASSIGNMENT ( #6706, #838, ( #4992 ) ) ;
#8389 = CARTESIAN_POINT ( 'NONE',  ( -0.7011654427748897911, 2.490287375297125294, -44.24552462515097062 ) ) ;
#8390 = CARTESIAN_POINT ( 'NONE',  ( 0.000000000000000000, 12.50000000000000178, 0.2499999999999998057 ) ) ;
#8391 = AXIS2_PLACEMENT_3D ( 'NONE', #2620, #7161, #8559 ) ;
#8392 = CARTESIAN_POINT ( 'NONE',  ( -63.22816877820476833, 10.40788280221283735, -203.5738002078235809 ) ) ;
#8393 = CARTESIAN_POINT ( 'NONE',  ( -3.249999999999999112, 1.812499999999999778, -4.846194077712558723 ) ) ;
#8394 = CARTESIAN_POINT ( 'NONE',  ( 10.75998892872498658, 2.667360448133907713, -106.5950482656118794 ) ) ;
#8395 = AXIS2_PLACEMENT_3D ( 'NONE', #9436, #7262, #4646 ) ;
#8396 = DATE_AND_TIME ( #3686, #4504 ) ;
#8397 = AXIS2_PLACEMENT_3D ( 'NONE', #8086, #15226, #5545 ) ;
#8398 = LINE ( 'NONE', #3618, #7494 ) ;
#8399 = CARTESIAN_POINT ( 'NONE',  ( -0.3766621274091715987, -0.2500000000000000000, -7.146945437571387671 ) ) ;
#8400 = ORIENTED_EDGE ( 'NONE', *, *, #7717, .T. ) ;
#8401 = CARTESIAN_POINT ( 'NONE',  ( 6.795064564604292201, 0.7174242581283463149, 3.395653431975275804 ) ) ;
#8402 = CARTESIAN_POINT ( 'NONE',  ( -3.249999999999999556, 1.312500000000000222, -4.846194077712557835 ) ) ;
#8403 = CARTESIAN_POINT ( 'NONE',  ( -68.72755137142191018, 10.00000000000000355, -180.2525548315512083 ) ) ;
#8404 = CARTESIAN_POINT ( 'NONE',  ( -1.346194077712558945, 0.5625000000000001110, -0.2500000000000002220 ) ) ;
#8405 = VECTOR ( 'NONE', #5848, 1000.000000000000000 ) ;
#8406 = CARTESIAN_POINT ( 'NONE',  ( -3.249999999999999112, 4.812500000000001776, -4.846194077712558723 ) ) ;
#8407 = VERTEX_POINT ( 'NONE', #3379 ) ;
#8408 = CARTESIAN_POINT ( 'NONE',  ( -1.167553989851729979, 15.00000000000000000, -119.2042076268937336 ) ) ;
#8409 = CARTESIAN_POINT ( 'NONE',  ( 0.2625675448779695720, 9.999999999999998224, 2.974107436473218957 ) ) ;
#8410 = CARTESIAN_POINT ( 'NONE',  ( -11.91260474549187798, 9.999999999999998224, -150.3549708560018132 ) ) ;
#8411 = CARTESIAN_POINT ( 'NONE',  ( 1.831246893856133928, -2.490287375297125294, -1.000000000000000888 ) ) ;
#8412 = CARTESIAN_POINT ( 'NONE',  ( -3.749999999999999556, 1.750000000000000000, -3.499999999999999112 ) ) ;
#8413 = CARTESIAN_POINT ( 'NONE',  ( 3.750000000000000000, 5.750000000000000000, -3.500000000000000444 ) ) ;
#8414 = CARTESIAN_POINT ( 'NONE',  ( -3.724891368794485125, 9.650666666666664284, -47.87745094654707145 ) ) ;
#8415 = CARTESIAN_POINT ( 'NONE',  ( -4.592425496802573972E-16, 6.000000000000000888, -7.250000000000000000 ) ) ;
#8416 = CARTESIAN_POINT ( 'NONE',  ( 1.518127423188106340, 13.34476997861058933, 4.548776429828005341 ) ) ;
#8417 = DIRECTION ( 'NONE',  ( -1.000000000000000000, 0.000000000000000000, 0.000000000000000000 ) ) ;
#8418 = CARTESIAN_POINT ( 'NONE',  ( 8.895558325401111688, 15.00000000000000000, -141.4560052469132643 ) ) ;
#8419 = B_SPLINE_CURVE_WITH_KNOTS ( 'NONE', 3,
 ( #14300, #6170, #3699, #9428, #9740, #7166, #5861, #10892, #308, #5022, #1389, #7251, #10580, #3865, #13141, #11968, #2551, #1310, #9572, #5938, #4937, #14154 ),
 .UNSPECIFIED., .F., .F.,
 ( 4, 2, 2, 2, 2, 2, 2, 2, 2, 2, 4 ),
 ( 5.421010862427521568E-20, 0.001104514646399055826, 0.002209029292798111652, 0.002761286615997639998, 0.003313543939197167477, 0.004418058585596228507, 0.005522573231995289537, 0.006627087878394349700, 0.007731602524793410730, 0.008283859847992942546, 0.008836117171192472627 ),
 .UNSPECIFIED. ) ;
#8420 = CARTESIAN_POINT ( 'NONE',  ( -8.765507753109435640, 1.591638444933427977E-16, -148.3002607745583816 ) ) ;
#8421 = CARTESIAN_POINT ( 'NONE',  ( -1.346194077712559389, 11.43750000000000000, -6.749999999999999112 ) ) ;
#8422 = CARTESIAN_POINT ( 'NONE',  ( 5.021457302209542561, 0.1001282284926883204, -1.279387354551734024 ) ) ;
#8423 = CARTESIAN_POINT ( 'NONE',  ( 6.122889832264990062, 9.999999999999998224, 5.281130614573720905 ) ) ;
#8424 = ORIENTED_EDGE ( 'NONE', *, *, #6940, .F. ) ;
#8425 = PRODUCT ( 'SmallSpring', 'SmallSpring', '', ( #14690 ) ) ;
#8426 = CARTESIAN_POINT ( 'NONE',  ( 1.553300858899105963, 10.06250000000000000, -7.250000000000000888 ) ) ;
#8427 = ORIENTED_EDGE ( 'NONE', *, *, #6499, .T. ) ;
#8428 = CARTESIAN_POINT ( 'NONE',  ( -5.191659272572687556, 2.500000000000000444, -112.0623128200284953 ) ) ;
#8429 = CARTESIAN_POINT ( 'NONE',  ( -22.96235718882280707, 8.673617379884035472E-16, -203.4902939858489788 ) ) ;
#8430 = CARTESIAN_POINT ( 'NONE',  ( -4.592425496802573972E-16, 9.500000000000000000, -7.249999999999999112 ) ) ;
#8431 = CARTESIAN_POINT ( 'NONE',  ( -1.553300858899106629, 4.562500000000000000, 0.2499999999999998335 ) ) ;
#8432 = CARTESIAN_POINT ( 'NONE',  ( 0.3766621274091715987, -0.2500000000000000000, 0.1491815183709511716 ) ) ;
#8433 = ORIENTED_EDGE ( 'NONE', *, *, #1280, .T. ) ;
#8434 = AXIS2_PLACEMENT_3D ( 'NONE', #14182, #1495, #30 ) ;
#8435 = CARTESIAN_POINT ( 'NONE',  ( 2.298097038856278029, 3.125000000000000444, -5.798097038856279362 ) ) ;
#8436 = EDGE_CURVE ( 'NONE', #5913, #1934, #7222, .T. ) ;
#8437 = EDGE_CURVE ( 'NONE', #10316, #8996, #7472, .T. ) ;
#8438 = CARTESIAN_POINT ( 'NONE',  ( -67.50271866717234559, 9.999999999999998224, -175.2102855837734978 ) ) ;
#8439 = DIRECTION ( 'NONE',  ( 0.000000000000000000, 1.000000000000000000, 0.000000000000000000 ) ) ;
#8440 = EDGE_CURVE ( 'NONE', #191, #14278, #2153, .T. ) ;
#8441 = CARTESIAN_POINT ( 'NONE',  ( -3.249999999999999556, 6.250000000000000000, -3.499999999999999556 ) ) ;
#8442 = DIRECTION ( 'NONE',  ( 0.000000000000000000, 0.000000000000000000, 1.000000000000000000 ) ) ;
#8443 = PRODUCT_DEFINITION_FORMATION_WITH_SPECIFIED_SOURCE ( 'ANY', '', #14121, .NOT_KNOWN. ) ;
#8444 = CARTESIAN_POINT ( 'NONE',  ( -0.1621610429705883094, -1.190394676226177737E-12, -136.1940307089123507 ) ) ;
#8445 = CARTESIAN_POINT ( 'NONE',  ( 15.55587903155823248, 5.000000000000000888, -128.0070267003170272 ) ) ;
#8446 = ORIENTED_EDGE ( 'NONE', *, *, #367, .T. ) ;
#8447 = DIRECTION ( 'NONE',  ( -0.9997619372588932851, 0.000000000000000000, -0.02181900108494707474 ) ) ;
#8448 = CARTESIAN_POINT ( 'NONE',  ( 2.298097038856278473, 14.62500000000000000, -5.798097038856279362 ) ) ;
#8449 = ORIENTED_EDGE ( 'NONE', *, *, #4138, .F. ) ;
#8450 = ORIENTED_EDGE ( 'NONE', *, *, #9130, .T. ) ;
#8451 = DIRECTION ( 'NONE',  ( 0.000000000000000000, 0.000000000000000000, -1.000000000000000000 ) ) ;
#8452 = CARTESIAN_POINT ( 'NONE',  ( -1.553300858899106629, 5.562500000000001776, 0.2500000000000002220 ) ) ;
#8453 = CIRCLE ( 'NONE', #1837, 5.000000000000000000 ) ;
#8454 = PRODUCT_DEFINITION ( 'UNKNOWN', '', #5003, #7575 ) ;
#8455 = CARTESIAN_POINT ( 'NONE',  ( -1.346194077712559167, 8.937500000000000000, -6.749999999999999112 ) ) ;
#8456 = ORIENTED_EDGE ( 'NONE', *, *, #6455, .T. ) ;
#8457 = CARTESIAN_POINT ( 'NONE',  ( -2.869987474717050624, -2.075239479414269894, -1.000000000000000888 ) ) ;
#8458 = CARTESIAN_POINT ( 'NONE',  ( 1.346194077712560944, 5.937500000000000000, -0.2500000000000010547 ) ) ;
#8459 = DIRECTION ( 'NONE',  ( 0.8674617751425296452, 0.000000000000000000, 0.4975038378410473472 ) ) ;
#8460 = EDGE_CURVE ( 'NONE', #933, #7952, #583, .T. ) ;
#8461 = CARTESIAN_POINT ( 'NONE',  ( 4.492499072540838689, 5.000000000000000000, -2.611025101989581820 ) ) ;
#8462 = CARTESIAN_POINT ( 'NONE',  ( -67.58382170693636226, 5.000000000000000888, -204.5178482451963191 ) ) ;
#8463 = AXIS2_PLACEMENT_3D ( 'NONE', #1922, #6789, #12660 ) ;
#8464 = ADVANCED_FACE ( 'NONE', ( #5697 ), #9180, .F. ) ;
#8465 = DATE_AND_TIME ( #12257, #14315 ) ;
#8466 = CARTESIAN_POINT ( 'NONE',  ( 14.32267195561841433, 12.49999999999999822, -126.6197849905234278 ) ) ;
#8467 = ORIENTED_EDGE ( 'NONE', *, *, #7527, .T. ) ;
#8468 = CARTESIAN_POINT ( 'NONE',  ( -1.346194077712559389, 1.437500000000000000, -6.749999999999999112 ) ) ;
#8469 = CARTESIAN_POINT ( 'NONE',  ( 5.376486659670670853, 0.000000000000000000, -45.55632290616389923 ) ) ;
#8470 = AXIS2_PLACEMENT_3D ( 'NONE', #3580, #9762, #11831 ) ;
#8471 = CIRCLE ( 'NONE', #4300, 6.999999999999950262 ) ;
#8472 = CARTESIAN_POINT ( 'NONE',  ( -3.750000000000000000, 14.81250000000000355, -5.053300858899105741 ) ) ;
#8473 = CARTESIAN_POINT ( 'NONE',  ( -67.61523983689153283, 11.65026692799600205, -203.8419816591213021 ) ) ;
#8474 = PLANE ( 'NONE',  #14123 ) ;
#8475 = CARTESIAN_POINT ( 'NONE',  ( -1.346194077712559167, 2.937500000000000444, -6.749999999999999112 ) ) ;
#8476 = CARTESIAN_POINT ( 'NONE',  ( 7.504172156237145508, 0.1516696207292601850, -105.5034272634598977 ) ) ;
#8477 = EDGE_CURVE ( 'NONE', #5038, #13240, #9014, .T. ) ;
#8478 = APPROVAL_STATUS ( 'not_yet_approved' ) ;
#8479 = CARTESIAN_POINT ( 'NONE',  ( -0.9850606648477213678, 15.00000000000000000, -125.5681744140592144 ) ) ;
#8480 = VECTOR ( 'NONE', #2164, 1000.000000000000000 ) ;
#8481 = AXIS2_PLACEMENT_3D ( 'NONE', #14072, #6731, #3248 ) ;
#8482 = CARTESIAN_POINT ( 'NONE',  ( -2.141054399116760543, 9.999999999999998224, -102.7251783244459631 ) ) ;
#8483 = AXIS2_PLACEMENT_3D ( 'NONE', #9142, #7758, #7979 ) ;
#8484 = ORIENTED_EDGE ( 'NONE', *, *, #2215, .F. ) ;
#8485 = CARTESIAN_POINT ( 'NONE',  ( 8.196277028564448841, 2.365617111222970692, 2.402449729030273762 ) ) ;
#8486 = CARTESIAN_POINT ( 'NONE',  ( -1.346194077712558945, 7.062500000000000000, -0.2500000000000002220 ) ) ;
#8487 = CARTESIAN_POINT ( 'NONE',  ( 0.000000000000000000, 0.000000000000000000, -0.5000000000000018874 ) ) ;
#8488 = CARTESIAN_POINT ( 'NONE',  ( 2.298097038856278473, 12.62500000000000000, -5.798097038856279362 ) ) ;
#8489 = CARTESIAN_POINT ( 'NONE',  ( 1.346194077712558279, 8.062500000000001776, -6.750000000000000888 ) ) ;
#8490 = CARTESIAN_POINT ( 'NONE',  ( -5.170287126184733850, 15.00000000000000000, -112.1835598689884108 ) ) ;
#8491 = FACE_OUTER_BOUND ( 'NONE', #1585, .T. ) ;
#8492 = CARTESIAN_POINT ( 'NONE',  ( -3.249999999999999556, 0.1875000000000000278, -2.153805922287440833 ) ) ;
#8493 = CIRCLE ( 'NONE', #12696, 4.999999999999992895 ) ;
#8494 = CARTESIAN_POINT ( 'NONE',  ( 3.749999999999999556, 1.249999999999999778, -3.500000000000000444 ) ) ;
#8495 = CARTESIAN_POINT ( 'NONE',  ( 2.651650429449552870, 5.625000000000000000, -6.151650429449554203 ) ) ;
#8496 = CARTESIAN_POINT ( 'NONE',  ( -3.691420245339825712, 15.00000000000000000, -128.6724311331325339 ) ) ;
#8497 = CARTESIAN_POINT ( 'NONE',  ( 0.000000000000000000, 4.499999999999999112, 0.2500000000000002220 ) ) ;
#8498 = CARTESIAN_POINT ( 'NONE',  ( 0.3534949980169243555, 11.00682189557416990, 2.912326207404907219 ) ) ;
#8499 = CARTESIAN_POINT ( 'NONE',  ( -4.022906649771232246, 11.02829952875353392, -46.76855065446253690 ) ) ;
#8500 = DIRECTION ( 'NONE',  ( 0.05964429961207245307, -0.000000000000000000, 0.9982196940171964572 ) ) ;
#8501 = CARTESIAN_POINT ( 'NONE',  ( 1.123966981038241109, 8.673617379884035472E-16, -145.3508939974056773 ) ) ;
#8502 = FACE_OUTER_BOUND ( 'NONE', #7929, .T. ) ;
#8503 = CARTESIAN_POINT ( 'NONE',  ( -22.33245550614446984, 8.673617379884035472E-16, -176.1180941298629818 ) ) ;
#8504 = CARTESIAN_POINT ( 'NONE',  ( -65.18383229995919237, 14.84510318562159448, -190.8261455846306660 ) ) ;
#8505 = EDGE_LOOP ( 'NONE', ( #13837, #13132, #13004, #2341 ) ) ;
#8506 = CARTESIAN_POINT ( 'NONE',  ( -1.553300858899106629, 9.562500000000000000, 0.2500000000000002220 ) ) ;
#8507 = ORIENTED_EDGE ( 'NONE', *, *, #2711, .T. ) ;
#8508 = CARTESIAN_POINT ( 'NONE',  ( -5.131649475085241718, 2.500000000000000444, -112.7947322869679709 ) ) ;
#8509 = CARTESIAN_POINT ( 'NONE',  ( -6.805338252203101845, -1.921202954650397476, -45.13192727926511338 ) ) ;
#8510 = CARTESIAN_POINT ( 'NONE',  ( -3.750000000000000000, 7.250000000000000000, -3.499999999999999112 ) ) ;
#8511 = CARTESIAN_POINT ( 'NONE',  ( -1.553300858899106629, 8.562500000000001776, 0.2499999999999998335 ) ) ;
#8512 = CARTESIAN_POINT ( 'NONE',  ( 22.93326999583280923, 1.750000000002257083, 28.81042027259682214 ) ) ;
#8513 = ORIENTED_EDGE ( 'NONE', *, *, #1728, .T. ) ;
#8514 = PERSON ( 'NAUO-PER5', 'UNSPECIFIED', 'UNSPECIFIED', ('UNSPECIFIED'), ('UNSPECIFIED'), ('UNSPECIFIED') ) ;
#8515 = CARTESIAN_POINT ( 'NONE',  ( -1.346194077712558945, 5.562500000000000000, -0.2500000000000002220 ) ) ;
#8516 = B_SPLINE_CURVE_WITH_KNOTS ( 'NONE', 3,
 ( #3073, #10329, #12500, #11337, #761, #1845, #15068, #6551, #1917, #6707 ),
 .UNSPECIFIED., .F., .F.,
 ( 4, 2, 2, 2, 4 ),
 ( 9.697399036122160616E-19, 0.0007311508082448070923, 0.001462301616489613100, 0.002193452424734419325, 0.002924603232979225333 ),
 .UNSPECIFIED. ) ;
#8517 = CARTESIAN_POINT ( 'NONE',  ( -3.749999999999999556, 9.312499999999998224, -5.053300858899104853 ) ) ;
#8518 = CARTESIAN_POINT ( 'NONE',  ( -64.24938361218754324, 15.00000000000000000, -199.4097214783338643 ) ) ;
#8519 = DIRECTION ( 'NONE',  ( -0.000000000000000000, 1.000000000000000000, -0.000000000000000000 ) ) ;
#8520 = DIRECTION ( 'NONE',  ( 1.000000000000000000, 0.000000000000000000, 0.000000000000000000 ) ) ;
#8521 = CARTESIAN_POINT ( 'NONE',  ( -2.298097038856278473, 8.125000000000000000, -1.201902961143720416 ) ) ;
#8522 = CARTESIAN_POINT ( 'NONE',  ( 0.5277094098148726875, 5.000000000000800249, -137.0293413729473571 ) ) ;
#8523 = CARTESIAN_POINT ( 'NONE',  ( 8.346107330767033261, -2.159485683299472295E-13, -114.8449120968014796 ) ) ;
#8524 = ORIENTED_EDGE ( 'NONE', *, *, #12426, .F. ) ;
#8525 = DIRECTION ( 'NONE',  ( 0.000000000000000000, 0.000000000000000000, 1.000000000000000000 ) ) ;
#8526 = CARTESIAN_POINT ( 'NONE',  ( 3.249999999999999556, 14.75000000000000178, -3.500000000000000000 ) ) ;
#8527 = ORIENTED_EDGE ( 'NONE', *, *, #4420, .F. ) ;
#8528 = VERTEX_POINT ( 'NONE', #3308 ) ;
#8529 = CARTESIAN_POINT ( 'NONE',  ( 23.72559141557340112, 0.5631470407087223462, -138.6353840888844502 ) ) ;
#8530 = CARTESIAN_POINT ( 'NONE',  ( -3.750000000000000000, 12.68750000000000178, -1.946699141100893149 ) ) ;
#8531 = CARTESIAN_POINT ( 'NONE',  ( 1.346194077712561166, 8.437500000000000000, -0.2500000000000011102 ) ) ;
#8532 = CARTESIAN_POINT ( 'NONE',  ( 2.298097038856278029, 10.12500000000000000, -5.798097038856279362 ) ) ;
#8533 = ORIENTED_EDGE ( 'NONE', *, *, #13980, .F. ) ;
#8534 = ADVANCED_FACE ( 'NONE', ( #9257 ), #4251, .F. ) ;
#8535 = CARTESIAN_POINT ( 'NONE',  ( -3.504378794273236508, 14.99999999999999822, -116.8541096786202331 ) ) ;
#8536 = CARTESIAN_POINT ( 'NONE',  ( -3.980102097228897245E-16, 6.500000000000000888, -6.749999999999999112 ) ) ;
#8537 = CARTESIAN_POINT ( 'NONE',  ( -7.950184983571356945, 9.999999999999994671, -122.1589960244479016 ) ) ;
#8538 = CARTESIAN_POINT ( 'NONE',  ( 9.304453467381463838, 4.110933237340877717E-16, -163.3650005149288233 ) ) ;
#8539 = CARTESIAN_POINT ( 'NONE',  ( -48.00729659322606580, 15.00000000000000178, -156.2075853427034247 ) ) ;
#8540 = APPROVAL_DATE_TIME ( #14446, #10653 ) ;
#8541 = CARTESIAN_POINT ( 'NONE',  ( 17.50071171097425804, 8.749999999999998224, -91.70093451412481045 ) ) ;
#8542 = ORIENTED_EDGE ( 'NONE', *, *, #3374, .T. ) ;
#8543 = CARTESIAN_POINT ( 'NONE',  ( -1.346194077712559389, 0.06250000000000000000, -0.2500000000000002220 ) ) ;
#8544 = CARTESIAN_POINT ( 'NONE',  ( 3.749999999999998668, 12.68750000000000178, -5.053300858899107517 ) ) ;
#8545 = EDGE_CURVE ( 'NONE', #273, #9933, #6986, .T. ) ;
#8546 = DIRECTION ( 'NONE',  ( 0.000000000000000000, 0.000000000000000000, 1.000000000000000000 ) ) ;
#8547 = CARTESIAN_POINT ( 'NONE',  ( -2.651650429449552870, 12.62500000000000000, -0.8483495705504467965 ) ) ;
#8548 = CARTESIAN_POINT ( 'NONE',  ( -65.52812891407587870, 15.29456201715631813, -203.7013355924380278 ) ) ;
#8549 = DIRECTION ( 'NONE',  ( 8.764770998266002131E-18, -0.000000000000000000, 1.000000000000000000 ) ) ;
#8550 = CARTESIAN_POINT ( 'NONE',  ( 2.298097038856279362, 1.375000000000000000, -1.201902961143720860 ) ) ;
#8551 = CARTESIAN_POINT ( 'NONE',  ( 10.79363737070329776, 14.04001088496077543, -106.2926778297471060 ) ) ;
#8552 = COORDINATED_UNIVERSAL_TIME_OFFSET ( 0, 0, .AHEAD. ) ;
#8553 = AXIS2_PLACEMENT_3D ( 'NONE', #9582, #13309, #9823 ) ;
#8554 = CARTESIAN_POINT ( 'NONE',  ( 4.371113732131426843, 2.850949024098341860E-47, -126.7907979241013408 ) ) ;
#8555 = LINE ( 'NONE', #14142, #4704 ) ;
#8556 = ORIENTED_EDGE ( 'NONE', *, *, #3673, .T. ) ;
#8557 = CARTESIAN_POINT ( 'NONE',  ( 5.630997345025299694, 2.457945380941962465, 4.493121576497173919 ) ) ;
#8558 = CARTESIAN_POINT ( 'NONE',  ( 3.249999999999999556, 5.750000000000000000, -3.500000000000000000 ) ) ;
#8559 = DIRECTION ( 'NONE',  ( 0.000000000000000000, 0.000000000000000000, -1.000000000000000000 ) ) ;
#8560 = CARTESIAN_POINT ( 'NONE',  ( -3.249999999999999556, 14.25000000000000000, -3.499999999999999556 ) ) ;
#8561 = EDGE_CURVE ( 'NONE', #8996, #10252, #3148, .T. ) ;
#8562 = CARTESIAN_POINT ( 'NONE',  ( -3.980102097228897738E-16, 8.999999999999998224, -6.749999999999999112 ) ) ;
#8563 = CARTESIAN_POINT ( 'NONE',  ( -0.9850606648477213678, 15.00000000000000000, -125.5681744140592144 ) ) ;
#8564 = CLOSED_SHELL ( 'NONE', ( #5471, #15100, #9992, #3352, #1257, #12816, #15077, #11401, #10263, #2144, #14148, #12451, #3832, #12509, #7546, #5002, #12711, #1647, #6962, #10188, #11834, #14702, #8464, #10186, #7804, #2973, #5886, #15215, #11210, #3741, #606, #279, #8367, #5633, #5617, #9102, #11969, #14144, #1965, #12599, #1966, #3527, #14725, #12889, #6676, #10837, #13962, #12734, #9192, #13834, #342, #11778, #9407, #6922, #9340, #2608, #12536, #6376, #14654, #1883, #9042, #5725, #8774, #8854, #137, #7862, #11963, #11317, #4986, #4325, #3431, #4692, #11734, #2072, #10953 ) ) ;
#8565 = ADVANCED_FACE ( 'NONE', ( #11342 ), #10946, .T. ) ;
#8566 = CARTESIAN_POINT ( 'NONE',  ( 0.000000000000000000, 1.000000000000000000, 0.000000000000000000 ) ) ;
#8567 = ADVANCED_FACE ( 'NONE', ( #9100 ), #11501, .T. ) ;
#8568 = CARTESIAN_POINT ( 'NONE',  ( 9.985652091690132792, 14.71651756310949999, -106.3014141697038042 ) ) ;
#8569 = CARTESIAN_POINT ( 'NONE',  ( -3.980102097228897245E-16, 4.500000000000000888, -6.749999999999999112 ) ) ;
#8570 = CARTESIAN_POINT ( 'NONE',  ( 3.249999999999999556, 15.25000000000000355, -3.500000000000000000 ) ) ;
#8571 = CARTESIAN_POINT ( 'NONE',  ( 2.651650429449552870, 6.625000000000000000, -6.151650429449554203 ) ) ;
#8572 = CARTESIAN_POINT ( 'NONE',  ( 0.2611203624075133511, 4.669981294363242164, 2.957715173867767167 ) ) ;
#8573 = CARTESIAN_POINT ( 'NONE',  ( 3.750000000000000000, 7.312500000000001776, -1.946699141100892705 ) ) ;
#8574 = CARTESIAN_POINT ( 'NONE',  ( 3.666659101104859264, 12.53633980302105755, 4.393427362251489221 ) ) ;
#8575 = CARTESIAN_POINT ( 'NONE',  ( 10.72774301836061639, 0.4980643078076283370, -164.7196873471209244 ) ) ;
#8576 = CARTESIAN_POINT ( 'NONE',  ( 24.11812047241811285, 4.000000000000000000, -143.1328717288817813 ) ) ;
#8577 = CARTESIAN_POINT ( 'NONE',  ( -17.32624372123753886, 15.00000000000000000, -122.3796757791585321 ) ) ;
#8578 = CARTESIAN_POINT ( 'NONE',  ( 3.249999999999999112, 14.81250000000000000, -2.153805922287439945 ) ) ;
#8579 = CARTESIAN_POINT ( 'NONE',  ( 1.401654536806489659, 8.673617379884035472E-16, -145.1626543382392924 ) ) ;
#8580 = CARTESIAN_POINT ( 'NONE',  ( 3.136841903360910067, 5.000000000000000888, -104.4936450199714812 ) ) ;
#8581 = VERTEX_POINT ( 'NONE', #7308 ) ;
#8582 = CARTESIAN_POINT ( 'NONE',  ( 3.750000000000000000, 13.31250000000000178, -1.946699141100892705 ) ) ;
#8583 = ORIENTED_EDGE ( 'NONE', *, *, #14635, .F. ) ;
#8584 = CARTESIAN_POINT ( 'NONE',  ( -6.654685603881863365, 7.806255641895631925E-15, -108.0058818677553774 ) ) ;
#8585 = CARTESIAN_POINT ( 'NONE',  ( -11.27598888897756702, -1.020558061026470176, -40.77697206847461331 ) ) ;
#8586 = CARTESIAN_POINT ( 'NONE',  ( -1.553300858899106629, 10.06250000000000000, 0.2500000000000002220 ) ) ;
#8587 = CARTESIAN_POINT ( 'NONE',  ( -1.553300858899107073, 6.937500000000001776, -7.249999999999999112 ) ) ;
#8588 = CARTESIAN_POINT ( 'NONE',  ( 9.044950117654433797, 0.000000000000000000, -144.9826476090360643 ) ) ;
#8589 = ORIENTED_EDGE ( 'NONE', *, *, #3152, .F. ) ;
#8590 = CARTESIAN_POINT ( 'NONE',  ( -9.486278975404857761, 3.140033110049585741, -115.8846352400757240 ) ) ;
#8591 = CARTESIAN_POINT ( 'NONE',  ( 2.298097038856278029, 4.125000000000000000, -5.798097038856279362 ) ) ;
#8592 = CARTESIAN_POINT ( 'NONE',  ( -3.750000000000000000, 11.25000000000000000, -3.499999999999999112 ) ) ;
#8593 = CARTESIAN_POINT ( 'NONE',  ( -61.28061730015007669, 15.00000000000000711, -159.7704501039084448 ) ) ;
#8594 = FACE_OUTER_BOUND ( 'NONE', #4154, .T. ) ;
#8595 =( NAMED_UNIT ( * ) PLANE_ANGLE_UNIT ( ) SI_UNIT ( $, .RADIAN. ) );
#8596 = CARTESIAN_POINT ( 'NONE',  ( -3.249999999999999556, 9.312499999999998224, -4.846194077712557835 ) ) ;
#8597 = APPROVAL_STATUS ( 'not_yet_approved' ) ;
#8598 = CARTESIAN_POINT ( 'NONE',  ( -3.672164062207812218, -6.326810776413004444E-12, -131.0905698957661514 ) ) ;
#8599 = CARTESIAN_POINT ( 'NONE',  ( 6.285553548860313811, 8.673617379884035472E-16, -104.9603685434299649 ) ) ;
#8600 = ORIENTED_EDGE ( 'NONE', *, *, #1584, .F. ) ;
#8601 = CARTESIAN_POINT ( 'NONE',  ( -8.205916711996726676, 7.499999999999991118, -92.94857034792688921 ) ) ;
#8602 = CARTESIAN_POINT ( 'NONE',  ( 26.15341798802279527, 4.000000000000000000, -138.7600702976168066 ) ) ;
#8603 = VERTEX_POINT ( 'NONE', #10789 ) ;
#8604 = ORIENTED_EDGE ( 'NONE', *, *, #5370, .T. ) ;
#8605 = CARTESIAN_POINT ( 'NONE',  ( -0.2515148708112424081, 0.2743742620810324939, -6.863050255469944183 ) ) ;
#8606 = CARTESIAN_POINT ( 'NONE',  ( 1.553300858899105963, 13.06250000000000178, -7.249999999999999112 ) ) ;
#8607 = CARTESIAN_POINT ( 'NONE',  ( 3.249999999999998224, 11.18750000000000178, -4.846194077712561388 ) ) ;
#8608 = AXIS2_PLACEMENT_3D ( 'NONE', #14789, #703, #12291 ) ;
#8609 = CARTESIAN_POINT ( 'NONE',  ( -3.249999999999999112, 9.812500000000000000, -4.846194077712558723 ) ) ;
#8610 = ORIENTED_EDGE ( 'NONE', *, *, #6941, .T. ) ;
#8611 = LINE ( 'NONE', #13268, #12179 ) ;
#8612 = CARTESIAN_POINT ( 'NONE',  ( 2.298097038856278473, 7.625000000000000000, -5.798097038856279362 ) ) ;
#8613 = FACE_OUTER_BOUND ( 'NONE', #5433, .T. ) ;
#8614 = CARTESIAN_POINT ( 'NONE',  ( -62.13313392481989439, 9.999999999999998224, -194.8801037569120069 ) ) ;
#8615 = CARTESIAN_POINT ( 'NONE',  ( 8.673617379884035472E-16, 5.000000000000000888, -1.663700395152567513 ) ) ;
#8616 = DATE_AND_TIME ( #14597, #1721 ) ;
#8617 = DIRECTION ( 'NONE',  ( 0.02181900108494707474, 0.000000000000000000, -0.9997619372588931741 ) ) ;
#8618 = ORIENTED_EDGE ( 'NONE', *, *, #5349, .F. ) ;
#8619 = CARTESIAN_POINT ( 'NONE',  ( 2.298097038856279362, 14.37500000000000000, -1.201902961143720860 ) ) ;
#8620 = CARTESIAN_POINT ( 'NONE',  ( 0.000000000000000000, 15.00000000000000000, 0.2500000000000002220 ) ) ;
#8621 = CARTESIAN_POINT ( 'NONE',  ( -4.422205167688408878, -1.921202954650395478, -0.5343376690911894045 ) ) ;
#8622 = CIRCLE ( 'NONE', #10858, 2.000000000000001776 ) ;
#8624 = CARTESIAN_POINT ( 'NONE',  ( -4.592425496802573972E-16, 2.500000000000000000, -7.249999999999999112 ) ) ;
#8623 =( BOUNDED_SURFACE ( )  B_SPLINE_SURFACE ( 3, 2, ( 
 ( #10721, #135, #682 ),
 ( #6467, #11183, #14989 ),
 ( #10258, #4163, #4387 ),
 ( #7784, #14688, #5388 ),
 ( #7704, #9094, #525 ),
 ( #13523, #1840, #14765 ),
 ( #7855, #1679, #11416 ),
 ( #835, #609, #5240 ),
 ( #13815, #5540, #1914 ),
 ( #6548, #11104, #7552 ),
 ( #12270, #4089, #2921 ),
 ( #7623, #8793, #1987 ),
 ( #6392, #8865, #6627 ),
 ( #12339, #9950, #1759 ),
 ( #5315, #10028, #11260 ),
 ( #14919, #2999, #8943 ),
 ( #13594, #12417, #10102 ),
 ( #14839, #4239, #13671 ),
 ( #12497, #3070, #11334 ),
 ( #757, #5467, #10184 ) ),
 .UNSPECIFIED., .F., .F., .T. ) 
 B_SPLINE_SURFACE_WITH_KNOTS ( ( 4, 2, 2, 2, 2, 2, 2, 2, 2, 4 ),
 ( 3, 3 ),
 ( 0.01021656723133482908, 0.01070697027993146831, 0.01095217180422978706, 0.01119737332852810754, 0.01168777637712474678, 0.01217817942572138601, 0.01266858247431802524, 0.01315898552291466447, 0.01364938857151130371, 0.01413979162010794294 ),
 ( 0.000000000000000000, 1.000000000000000000 ),
 .UNSPECIFIED. ) 
 GEOMETRIC_REPRESENTATION_ITEM ( )  RATIONAL_B_SPLINE_SURFACE ( (
 ( 1.000000000000000000, 0.6693962893781482126, 1.000000000000000000),
 ( 1.000000000000000000, 0.6693971655676271837, 1.000000000000000000),
 ( 1.000000000000000000, 0.6695055079298116718, 1.000000000000000000),
 ( 1.000000000000000000, 0.6698470843657819973, 1.000000000000000000),
 ( 1.000000000000000000, 0.6699916310626345961, 1.000000000000000000),
 ( 1.000000000000000000, 0.6703393818075829014, 1.000000000000000000),
 ( 1.000000000000000000, 0.6705430798865028574, 1.000000000000000000),
 ( 1.000000000000000000, 0.6712520209205289357, 1.000000000000000000),
 ( 1.000000000000000000, 0.6718564003725113754, 1.000000000000000000),
 ( 1.000000000000000000, 0.6734024997055334527, 1.000000000000000000),
 ( 1.000000000000000000, 0.6743323796560330985, 1.000000000000000000),
 ( 1.000000000000000000, 0.6766315243239030552, 1.000000000000000000),
 ( 1.000000000000000000, 0.6779734166346523816, 1.000000000000000000),
 ( 1.000000000000000000, 0.6812445256750346845, 1.000000000000000000),
 ( 1.000000000000000000, 0.6831973919983876931, 1.000000000000000000),
 ( 1.000000000000000000, 0.6879353199740830815, 1.000000000000000000),
 ( 1.000000000000000000, 0.6907034268515229725, 1.000000000000000000),
 ( 1.000000000000000000, 0.6976421491555230281, 1.000000000000000000),
 ( 1.000000000000000000, 0.7018548256397145746, 1.000000000000000000),
 ( 1.000000000000000000, 0.7071067811865475727, 1.000000000000000000) ) ) 
 REPRESENTATION_ITEM ( '' )  SURFACE ( )  );
#8625 = CARTESIAN_POINT ( 'NONE',  ( -67.60114792446165666, 11.17285071187519385, -204.1860880824393405 ) ) ;
#8626 = DIRECTION ( 'NONE',  ( 1.000000000000000000, 0.000000000000000000, 0.000000000000000000 ) ) ;
#8627 = EDGE_CURVE ( 'NONE', #8296, #13571, #7329, .T. ) ;
#8628 = CARTESIAN_POINT ( 'NONE',  ( 11.32016196459919399, 5.000000000000001776, -106.4092894470421271 ) ) ;
#8629 = PERSON_AND_ORGANIZATION_ROLE ( 'creator' ) ;
#8630 = APPROVAL_PERSON_ORGANIZATION ( #1203, #4538, #7002 ) ;
#8631 = EDGE_CURVE ( 'NONE', #14015, #1063, #13202, .T. ) ;
#8632 = CARTESIAN_POINT ( 'NONE',  ( -8.289881740238500996, 2.529993217055223287, -35.21986562831451550 ) ) ;
#8633 = DIRECTION ( 'NONE',  ( 0.000000000000000000, 1.000000000000000000, 0.000000000000000000 ) ) ;
#8634 = CIRCLE ( 'NONE', #4928, 3.500000000000003109 ) ;
#8635 = EDGE_LOOP ( 'NONE', ( #250, #10543 ) ) ;
#8636 = CARTESIAN_POINT ( 'NONE',  ( 6.415040636403542607, 0.6340196072765523772, 1.032023330731489219 ) ) ;
#8637 = CARTESIAN_POINT ( 'NONE',  ( 2.298097038856278473, 5.625000000000000000, -5.798097038856279362 ) ) ;
#8638 = CARTESIAN_POINT ( 'NONE',  ( -8.570785970181212576, 1.189964233097702939, -105.3070837849071353 ) ) ;
#8639 = CARTESIAN_POINT ( 'NONE',  ( 3.249999999999999112, 13.81250000000000000, -2.153805922287439945 ) ) ;
#8640 = CARTESIAN_POINT ( 'NONE',  ( -2.298097038856278029, 10.62500000000000000, -1.201902961143720638 ) ) ;
#8641 = CARTESIAN_POINT ( 'NONE',  ( 9.044950117654433797, 4.000000000000000000, -144.9826476090360643 ) ) ;
#8642 = CARTESIAN_POINT ( 'NONE',  ( 3.249999999999999112, 0.8125000000000001110, -2.153805922287439945 ) ) ;
#8643 = ORGANIZATION ( 'NAUO-ORG7', 'UNSPECIFIED', 'UNSPECIFIED' ) ;
#8644 = DIRECTION ( 'NONE',  ( 0.000000000000000000, 0.000000000000000000, 1.000000000000000000 ) ) ;
#8645 = CARTESIAN_POINT ( 'NONE',  ( -3.249999999999999556, 6.250000000000000000, -3.499999999999999556 ) ) ;
#8646 = CARTESIAN_POINT ( 'NONE',  ( -2.651650429449552870, 6.875000000000000000, -6.151650429449552426 ) ) ;
#8647 = CIRCLE ( 'NONE', #8395, 3.250000000000005329 ) ;
#8648 = AXIS2_PLACEMENT_3D ( 'NONE', #12197, #10107, #1685 ) ;
#8649 = CARTESIAN_POINT ( 'NONE',  ( -3.750000000000000000, 10.31250000000000000, -5.053300858899105741 ) ) ;
#8650 = B_SPLINE_CURVE_WITH_KNOTS ( 'NONE', 3,
 ( #13378, #13607, #11197, #7486, #1620, #4172, #13458, #14700, #7562, #3010, #11423, #987, #15152, #5619, #11649, #12582, #14851, #1996 ),
 .UNSPECIFIED., .F., .F.,
 ( 4, 2, 2, 2, 2, 2, 2, 2, 4 ),
 ( 0.000000000000000000, 0.002234240643988127332, 0.003351360965982170398, 0.004468481287976213898, 0.006702721931964300030, 0.008936962575952387897, 0.01117120321994047663, 0.01340544386392856363, 0.01787392515190473763 ),
 .UNSPECIFIED. ) ;
#8651 = CARTESIAN_POINT ( 'NONE',  ( -4.211572975458966361, 9.962993690351991560, -47.49266443388843584 ) ) ;
#8652 = CARTESIAN_POINT ( 'NONE',  ( 1.553300858899109516, 5.437500000000000888, 0.2499999999999993616 ) ) ;
#8653 = CARTESIAN_POINT ( 'NONE',  ( 1.598485290837698969, 13.49296761261617661, 1.982191991666128361 ) ) ;
#8654 = CARTESIAN_POINT ( 'NONE',  ( -8.289881740238515206, -2.075239479414269894, -35.21986562831452261 ) ) ;
#8655 = ADVANCED_FACE ( 'NONE', ( #10638 ), #13977, .F. ) ;
#8656 = EDGE_CURVE ( 'NONE', #10108, #8528, #10497, .T. ) ;
#8657 = CARTESIAN_POINT ( 'NONE',  ( 18.44985294524427388, 0.000000000000000000, 26.15777747556342803 ) ) ;
#8658 = CIRCLE ( 'NONE', #3990, 2.500000000000000000 ) ;
#8659 = CARTESIAN_POINT ( 'NONE',  ( -7.585720900221621932, 8.673617379884034486E-16, -147.1779900946870896 ) ) ;
#8660 = CARTESIAN_POINT ( 'NONE',  ( 5.940997791171045428, 0.02470368953922983876, -139.8438714080451462 ) ) ;
#8661 = AXIS2_PLACEMENT_3D ( 'NONE', #13564, #10075, #7525 ) ;
#8662 = AXIS2_PLACEMENT_3D ( 'NONE', #10587, #6024, #2561 ) ;
#8663 = CARTESIAN_POINT ( 'NONE',  ( -25.01903476313728447, 8.673617379884033500E-16, -185.3139711507751599 ) ) ;
#8664 = ORIENTED_EDGE ( 'NONE', *, *, #4956, .T. ) ;
#8665 = CARTESIAN_POINT ( 'NONE',  ( 2.651650429449554203, 14.37500000000000000, -0.8483495705504471296 ) ) ;
#8666 = VERTEX_POINT ( 'NONE', #10717 ) ;
#8667 = CARTESIAN_POINT ( 'NONE',  ( -65.53364736412717662, 5.000000000000000000, -203.4171941195418754 ) ) ;
#8668 = CARTESIAN_POINT ( 'NONE',  ( -15.87132822948224486, -8.950197302265710935E-13, -192.3250264793432507 ) ) ;
#8669 = CARTESIAN_POINT ( 'NONE',  ( -2.651650429449552870, 8.125000000000000000, -0.8483495705504462414 ) ) ;
#8670 = CARTESIAN_POINT ( 'NONE',  ( 1.553300858899105963, 7.062499999999999112, -7.249999999999999112 ) ) ;
#8671 = CARTESIAN_POINT ( 'NONE',  ( -3.421798459318232677, 10.60800287581505508, -46.00651939675768176 ) ) ;
#8672 = ORIENTED_EDGE ( 'NONE', *, *, #5538, .T. ) ;
#8673 = CARTESIAN_POINT ( 'NONE',  ( -3.249999999999999112, 3.687500000000000444, -2.153805922287440833 ) ) ;
#8674 = CIRCLE ( 'NONE', #7685, 3.500000000000000000 ) ;
#8675 = CARTESIAN_POINT ( 'NONE',  ( 3.749999999999999112, 11.81249999999999822, -1.946699141100892039 ) ) ;
#8676 = CARTESIAN_POINT ( 'NONE',  ( -69.84691631978306248, 15.00000000000114575, -196.7709020263189643 ) ) ;
#8677 = DIRECTION ( 'NONE',  ( -0.000000000000000000, 1.000000000000000000, 0.000000000000000000 ) ) ;
#8678 = COORDINATED_UNIVERSAL_TIME_OFFSET ( 0, 0, .AHEAD. ) ;
#8679 = CARTESIAN_POINT ( 'NONE',  ( 3.249999999999999112, 9.812500000000000000, -2.153805922287439945 ) ) ;
#8680 = EDGE_CURVE ( 'NONE', #11140, #13718, #13039, .T. ) ;
#8681 = CARTESIAN_POINT ( 'NONE',  ( -9.210337242589636375, 10.00000000000081535, -118.3325445942146246 ) ) ;
#8682 = CARTESIAN_POINT ( 'NONE',  ( -3.903074397104974391, 8.673617379884035472E-16, -118.5654830222526499 ) ) ;
#8683 = CARTESIAN_POINT ( 'NONE',  ( 8.518838221584619674, 8.673617379884035472E-16, -111.8377054444463141 ) ) ;
#8684 = ORIENTED_EDGE ( 'NONE', *, *, #4662, .F. ) ;
#8685 = CARTESIAN_POINT ( 'NONE',  ( -3.520407287333055635, 7.379999999999995453, -45.56125597433126018 ) ) ;
#8686 = CARTESIAN_POINT ( 'NONE',  ( 4.999884908348398049, 0.09438068890155060231, -1.653151978968578462 ) ) ;
#8687 = AXIS2_PLACEMENT_3D ( 'NONE', #10794, #208, #10959 ) ;
#8688 = ORIENTED_EDGE ( 'NONE', *, *, #8437, .F. ) ;
#8689 = DIRECTION ( 'NONE',  ( 0.000000000000000000, 0.000000000000000000, -1.000000000000000000 ) ) ;
#8690 = DIRECTION ( 'NONE',  ( 8.673617379884027583E-16, 0.000000000000000000, -1.000000000000000000 ) ) ;
#8691 = CARTESIAN_POINT ( 'NONE',  ( 3.749999999999998668, 11.18750000000000178, -5.053300858899108405 ) ) ;
#8692 = CARTESIAN_POINT ( 'NONE',  ( -2.298097038856279362, 12.87500000000000178, -5.798097038856278473 ) ) ;
#8693 = CARTESIAN_POINT ( 'NONE',  ( 2.298097038856279362, 11.37500000000000000, -1.201902961143720860 ) ) ;
#8694 = EDGE_LOOP ( 'NONE', ( #13829, #6604, #7677, #4885 ) ) ;
#8695 = DIRECTION ( 'NONE',  ( -0.000000000000000000, 1.000000000000000000, -0.000000000000000000 ) ) ;
#8696 = CARTESIAN_POINT ( 'NONE',  ( -2.298097038856278918, 8.375000000000000000, -5.798097038856277585 ) ) ;
#8697 = DIRECTION ( 'NONE',  ( 0.6527336816407245390, 0.000000000000000000, -0.7575874476598363216 ) ) ;
#8698 = LOCAL_TIME ( 12, 28, 20.00000000000000000, #14459 ) ;
#8699 = CARTESIAN_POINT ( 'NONE',  ( -8.484329074657676273, 2.500000000000001776, -105.8548167551525836 ) ) ;
#8700 = DIRECTION ( 'NONE',  ( -0.08794243244722436958, 0.000000000000000000, -0.9961255586397055328 ) ) ;
#8701 = DIRECTION ( 'NONE',  ( 0.002879925520667554837, 0.000000000000000000, 0.9999958530058988826 ) ) ;
#8702 = PERSON_AND_ORGANIZATION ( #3176, #3020 ) ;
#8703 = CARTESIAN_POINT ( 'NONE',  ( -25.01864811757476303, 1.587607347591324158, -206.7381864276124190 ) ) ;
#8704 = ORIENTED_EDGE ( 'NONE', *, *, #6474, .F. ) ;
#8705 = CARTESIAN_POINT ( 'NONE',  ( -3.249999999999999556, 0.2500000000000000000, -3.499999999999999556 ) ) ;
#8706 = CARTESIAN_POINT ( 'NONE',  ( -2.651650429449552870, -0.3749999999999998890, -0.8483495705504463524 ) ) ;
#8707 = ORIENTED_EDGE ( 'NONE', *, *, #1294, .T. ) ;
#8708 = CARTESIAN_POINT ( 'NONE',  ( 2.159942170319879562, 15.00000000000000000, -121.5147849362692369 ) ) ;
#8709 = CARTESIAN_POINT ( 'NONE',  ( 1.553300858899109071, 15.43750000000000178, 0.2499999999999989175 ) ) ;
#8710 = TOROIDAL_SURFACE ( 'NONE', #9710, 4.000000000000001776, 1.000000000000000000 ) ;
#8711 = DIRECTION ( 'NONE',  ( -0.000000000000000000, 1.000000000000000000, -0.000000000000000000 ) ) ;
#8712 = CARTESIAN_POINT ( 'NONE',  ( -9.385448347264265578, 5.000000000000000888, -115.3551636530117150 ) ) ;
#8713 = CARTESIAN_POINT ( 'NONE',  ( 3.750000000000000000, 1.750000000000000000, -3.500000000000000444 ) ) ;
#8714 = CALENDAR_DATE ( 2026, 8, 10 ) ;
#8715 = CARTESIAN_POINT ( 'NONE',  ( -64.90982034444132864, 14.98923205054743946, -184.4898348768445544 ) ) ;
#8716 = CARTESIAN_POINT ( 'NONE',  ( 2.159942170319879562, 5.000000000000000888, -121.5147849362692369 ) ) ;
#8717 = ORIENTED_EDGE ( 'NONE', *, *, #4680, .F. ) ;
#8718 = CARTESIAN_POINT ( 'NONE',  ( 1.346194077712558279, 8.562500000000000000, -6.750000000000000000 ) ) ;
#8719 = CIRCLE ( 'NONE', #14675, 2.000000000000000000 ) ;
#8720 = DIRECTION ( 'NONE',  ( 0.000000000000000000, 0.000000000000000000, 1.000000000000000000 ) ) ;
#8721 = AXIS2_PLACEMENT_3D ( 'NONE', #8298, #11707, #12875 ) ;
#8722 = CARTESIAN_POINT ( 'NONE',  ( 1.346194077712560944, 13.93750000000000000, -0.2500000000000010547 ) ) ;
#8723 = CARTESIAN_POINT ( 'NONE',  ( 3.249999999999998224, 12.31250000000000178, -2.153805922287439945 ) ) ;
#8724 = CARTESIAN_POINT ( 'NONE',  ( -1.724164254788412842, 7.321094445766562764, -19.52964039877223712 ) ) ;
#8725 =( BOUNDED_SURFACE ( )  B_SPLINE_SURFACE ( 3, 2, ( 
 ( #14470, #14155, #1462 ),
 ( #2703, #1229, #78 ),
 ( #2394, #13223, #10893 ),
 ( #9429, #3866, #309 ),
 ( #4862, #8568, #7403 ),
 ( #12127, #9504, #10738 ),
 ( #3701, #13142, #14701 ),
 ( #465, #4023, #7637 ),
 ( #10973, #5100, #5399 ),
 ( #1544, #6559, #11271 ),
 ( #12353, #10113, #693 ),
 ( #621, #391, #4252 ),
 ( #6403, #1854, #9814 ),
 ( #5178, #7563, #14853 ) ),
 .UNSPECIFIED., .F., .F., .T. ) 
 B_SPLINE_SURFACE_WITH_KNOTS ( ( 4, 2, 2, 2, 2, 2, 4 ),
 ( 3, 3 ),
 ( -9.470303715793572266E-06, 0.0005986386120071484880, 0.0009026930698686195555, 0.001206747527730090514, 0.001510801985591561473, 0.001814856443453032649, 0.002422965359175974567 ),
 ( 0.000000000000000000, 1.000000000000000000 ),
 .UNSPECIFIED. ) 
 GEOMETRIC_REPRESENTATION_ITEM ( )  RATIONAL_B_SPLINE_SURFACE ( (
 ( 1.000000000000000000, 1.000000000000000000, 1.000000000000000000),
 ( 1.000000000000000000, 1.000023086200706457, 1.000000000000000000),
 ( 1.000000000000000000, 0.9968203200712785206, 1.000000000000000000),
 ( 1.000000000000000000, 0.9876439521679505340, 1.000000000000000000),
 ( 1.000000000000000000, 0.9839375215982008038, 1.000000000000000000),
 ( 1.000000000000000000, 0.9755509977066852967, 1.000000000000000000),
 ( 1.000000000000000000, 0.9708179905542198007, 1.000000000000000000),
 ( 1.000000000000000000, 0.9610203602157827429, 1.000000000000000000),
 ( 1.000000000000000000, 0.9560186120561716683, 1.000000000000000000),
 ( 1.000000000000000000, 0.9464213852071460265, 1.000000000000000000),
 ( 1.000000000000000000, 0.9417776319690466247, 1.000000000000000000),
 ( 1.000000000000000000, 0.9300548202764272743, 1.000000000000000000),
 ( 1.000000000000000000, 0.9250790184741459754, 1.000000000000000000),
 ( 1.000000000000000000, 0.9251337988227811282, 1.000000000000000000) ) ) 
 REPRESENTATION_ITEM ( '' )  SURFACE ( )  );
#8726 = CARTESIAN_POINT ( 'NONE',  ( -65.53364736412717662, 5.000000000000000000, -203.4171941195418754 ) ) ;
#8727 = CARTESIAN_POINT ( 'NONE',  ( -2.869987474717051068, -2.075239479414269894, -1.000000000000004441 ) ) ;
#8728 = ADVANCED_FACE ( 'NONE', ( #5992 ), #12415, .F. ) ;
#8729 = CARTESIAN_POINT ( 'NONE',  ( -1.346194077712559389, 6.437500000000000888, -6.749999999999999112 ) ) ;
#8730 = CARTESIAN_POINT ( 'NONE',  ( 3.749999999999999112, 6.312500000000000000, -1.946699141100893149 ) ) ;
#8731 = CARTESIAN_POINT ( 'NONE',  ( -2.651650429449552870, 9.125000000000000000, -0.8483495705504462414 ) ) ;
#8732 = DIRECTION ( 'NONE',  ( 0.000000000000000000, 0.000000000000000000, 1.000000000000000000 ) ) ;
#8733 = CARTESIAN_POINT ( 'NONE',  ( -3.805829833685401287, 11.11844615798745828, -44.54564306111133476 ) ) ;
#8734 = CARTESIAN_POINT ( 'NONE',  ( 3.749999999999999556, 11.25000000000000000, -3.500000000000000444 ) ) ;
#8735 = VECTOR ( 'NONE', #5099, 1000.000000000000000 ) ;
#8736 = LINE ( 'NONE', #7802, #5994 ) ;
#8737 = CIRCLE ( 'NONE', #14677, 1.771449424009377438 ) ;
#8738 = CARTESIAN_POINT ( 'NONE',  ( 11.49434807426983340, 0.9346580912065771685, -164.9697452992295155 ) ) ;
#8739 = CARTESIAN_POINT ( 'NONE',  ( 19.54788354410667139, 2.100000000000000089, 25.09616337804641972 ) ) ;
#8740 = CARTESIAN_POINT ( 'NONE',  ( -25.59366506200112212, 8.673617379884035472E-16, -196.2657947609912696 ) ) ;
#8741 = DIRECTION ( 'NONE',  ( 0.1564344650402314796, 0.000000000000000000, 0.9876883405951375483 ) ) ;
#8742 = CARTESIAN_POINT ( 'NONE',  ( 5.578155699418820390, 0.2507831308262787329, 0.07728901913012563296 ) ) ;
#8743 = CARTESIAN_POINT ( 'NONE',  ( -3.249999999999999112, 0.6875000000000000000, -2.153805922287440833 ) ) ;
#8744 = VERTEX_POINT ( 'NONE', #4621 ) ;
#8745 = DIRECTION ( 'NONE',  ( 0.000000000000000000, 0.000000000000000000, -1.000000000000000000 ) ) ;
#8746 = PLANE ( 'NONE',  #6004 ) ;
#8747 = CARTESIAN_POINT ( 'NONE',  ( -3.749999999999999556, 9.187500000000000000, -1.946699141100892927 ) ) ;
#8748 = CIRCLE ( 'NONE', #13941, 1.000000000000042633 ) ;
#8749 = CARTESIAN_POINT ( 'NONE',  ( -1.553300858899106629, 6.562500000000000888, 0.2499999999999998335 ) ) ;
#8750 = DIRECTION ( 'NONE',  ( 0.000000000000000000, 0.000000000000000000, -1.000000000000000000 ) ) ;
#8751 = ORIENTED_EDGE ( 'NONE', *, *, #14614, .F. ) ;
#8752 = EDGE_CURVE ( 'NONE', #15312, #411, #2374, .T. ) ;
#8753 = CARTESIAN_POINT ( 'NONE',  ( -8.611029641430635095, 2.324435220029751559, -115.7034661592633995 ) ) ;
#8754 = CARTESIAN_POINT ( 'NONE',  ( -3.980102097228897738E-16, 7.000000000000000000, -6.749999999999999112 ) ) ;
#8755 = ADVANCED_FACE ( 'NONE', ( #2302 ), #2320, .F. ) ;
#8756 = CARTESIAN_POINT ( 'NONE',  ( 0.000000000000000000, 10.00000000000000000, 0.2500000000000002220 ) ) ;
#8757 = LINE ( 'NONE', #5423, #14102 ) ;
#8758 = CARTESIAN_POINT ( 'NONE',  ( 8.475206276408092876, 1.020558061026468177, -34.56909192082981974 ) ) ;
#8759 = DIRECTION ( 'NONE',  ( 0.000000000000000000, 0.000000000000000000, 1.000000000000000000 ) ) ;
#8760 = CARTESIAN_POINT ( 'NONE',  ( 1.346194077712560944, 12.93750000000000000, -0.2500000000000010547 ) ) ;
#8761 = AXIS2_PLACEMENT_3D ( 'NONE', #2108, #235, #1324 ) ;
#8762 = CARTESIAN_POINT ( 'NONE',  ( 7.352489943804304318, 2.529993217055222399, -39.38380306805898101 ) ) ;
#8763 = CARTESIAN_POINT ( 'NONE',  ( 0.5277094143303744378, -8.082121701904429344E-13, -137.0293413685615462 ) ) ;
#8764 = CARTESIAN_POINT ( 'NONE',  ( 9.719609032732419607, 5.000000000000000888, -108.8314952391709767 ) ) ;
#8765 = CARTESIAN_POINT ( 'NONE',  ( -0.2500000000000000555, 4.500000000000000888, 1.500000000000000222 ) ) ;
#8766 = CARTESIAN_POINT ( 'NONE',  ( 11.03716979879487425, 8.773889247172311556, -47.61077750239103779 ) ) ;
#8767 = ORIENTED_EDGE ( 'NONE', *, *, #11118, .F. ) ;
#8768 = CARTESIAN_POINT ( 'NONE',  ( 9.991517632468019272, 4.874398275619288512, -45.52987401239477805 ) ) ;
#8769 = CARTESIAN_POINT ( 'NONE',  ( 24.68832053908537461, 1.068321173883799435, -138.5167654850991141 ) ) ;
#8770 = CARTESIAN_POINT ( 'NONE',  ( -4.592425496802573972E-16, 13.00000000000000000, -7.250000000000000000 ) ) ;
#8771 = CARTESIAN_POINT ( 'NONE',  ( -3.249999999999999112, 10.81250000000000000, -4.846194077712558723 ) ) ;
#8772 = CARTESIAN_POINT ( 'NONE',  ( 3.249999999999999556, 0.7500000000000000000, -3.500000000000000000 ) ) ;
#8773 = ORIENTED_EDGE ( 'NONE', *, *, #10561, .F. ) ;
#8774 = ADVANCED_FACE ( 'NONE', ( #6237 ), #8710, .F. ) ;
#8775 = CARTESIAN_POINT ( 'NONE',  ( -2.298097038856278473, 12.12500000000000000, -1.201902961143720416 ) ) ;
#8776 = EDGE_CURVE ( 'NONE', #505, #12985, #14665, .T. ) ;
#8777 = ADVANCED_FACE ( 'NONE', ( #1444 ), #6388, .T. ) ;
#8778 = FACE_OUTER_BOUND ( 'NONE', #1193, .T. ) ;
#8779 = APPLICATION_CONTEXT ( 'configuration controlled 3d designs of mechanical parts and assemblies' ) ;
#8780 = CARTESIAN_POINT ( 'NONE',  ( 1.041485463413605039, 5.000000000000000888, -139.4527924098652534 ) ) ;
#8781 = CARTESIAN_POINT ( 'NONE',  ( 6.122889832264996279, 4.584371499408331552, 5.281130614573727122 ) ) ;
#8782 = CARTESIAN_POINT ( 'NONE',  ( -4.234402844927157794, 15.00000000000000000, -117.4888040839639558 ) ) ;
#8783 = APPROVAL_DATE_TIME ( #10244, #10179 ) ;
#8784 = CARTESIAN_POINT ( 'NONE',  ( -25.22236287666808607, 7.173903195122934007E-14, -199.9119606112305689 ) ) ;
#8785 = ORIENTED_EDGE ( 'NONE', *, *, #4780, .F. ) ;
#8786 = CARTESIAN_POINT ( 'NONE',  ( 1.346194077712560944, 0.9374999999999998890, -0.2500000000000010547 ) ) ;
#8787 = CARTESIAN_POINT ( 'NONE',  ( 0.000000000000000000, 13.00000000000000178, 0.2500000000000002220 ) ) ;
#8788 = EDGE_LOOP ( 'NONE', ( #7057, #39, #8688, #13871 ) ) ;
#8789 = CARTESIAN_POINT ( 'NONE',  ( 0.000000000000000000, 4.000000000000000000, 0.000000000000000000 ) ) ;
#8790 = CARTESIAN_POINT ( 'NONE',  ( -2.651650429449553314, 2.375000000000000000, -6.151650429449552426 ) ) ;
#8791 = PRODUCT_RELATED_PRODUCT_CATEGORY ( 'detail', '', ( #3617 ) ) ;
#8792 = CARTESIAN_POINT ( 'NONE',  ( 13.47730208875211844, 6.000000000000000000, -127.1728814958210876 ) ) ;
#8793 = CARTESIAN_POINT ( 'NONE',  ( 0.3429446965881275955, 1.040318156481846001, 3.884540920300163958 ) ) ;
#8794 = CARTESIAN_POINT ( 'NONE',  ( 3.749999999999999112, 2.687500000000000444, -5.053300858899108405 ) ) ;
#8795 = PERSON_AND_ORGANIZATION ( #3176, #3020 ) ;
#8796 = CARTESIAN_POINT ( 'NONE',  ( -2.837468109123920890, 2.075239479414269894, -0.7946808062301163877 ) ) ;
#8797 = DIRECTION ( 'NONE',  ( -0.3090169943749621062, 0.000000000000000000, -0.9510565162951489793 ) ) ;
#8798 = VERTEX_POINT ( 'NONE', #10870 ) ;
#8799 = CARTESIAN_POINT ( 'NONE',  ( 2.298097038856279362, 9.875000000000000000, -1.201902961143720860 ) ) ;
#8800 = CARTESIAN_POINT ( 'NONE',  ( -1.500000000000000000, 4.500000000000000888, -0.2499999999999997780 ) ) ;
#8801 = CARTESIAN_POINT ( 'NONE',  ( 3.249999999999999556, 4.249999999999999112, -3.500000000000000000 ) ) ;
#8802 = CARTESIAN_POINT ( 'NONE',  ( -1.346194077712559167, 11.93750000000000178, -6.749999999999999112 ) ) ;
#8803 = CARTESIAN_POINT ( 'NONE',  ( -7.575942540335539377, 15.00000000000153122, -106.7905032256090294 ) ) ;
#8804 = CARTESIAN_POINT ( 'NONE',  ( 1.123679064339592859, 4.590773665857039276, -139.4222662838609210 ) ) ;
#8805 = CARTESIAN_POINT ( 'NONE',  ( 3.249999999999998668, 5.687500000000000000, -4.846194077712560500 ) ) ;
#8806 = CARTESIAN_POINT ( 'NONE',  ( 0.000000000000000000, 5.500000000000000000, 0.2499999999999998057 ) ) ;
#8807 = CARTESIAN_POINT ( 'NONE',  ( 3.750000000000000000, 9.750000000000000000, -3.500000000000000444 ) ) ;
#8808 = CARTESIAN_POINT ( 'NONE',  ( 10.93997309537930285, 12.49999999999999822, -43.15715636164252089 ) ) ;
#8809 = CARTESIAN_POINT ( 'NONE',  ( 30.32986759126112730, 1.750000000000000000, 39.54214087805579680 ) ) ;
#8810 = CARTESIAN_POINT ( 'NONE',  ( -1.553300858899106629, 9.562500000000000000, 0.2500000000000002220 ) ) ;
#8811 = CARTESIAN_POINT ( 'NONE',  ( 4.374104445797671659, 15.00089282178949013, -1.804052482945163405 ) ) ;
#8812 = CARTESIAN_POINT ( 'NONE',  ( 10.88783379353840353, 0.4980643078046000372, -164.5252078881505327 ) ) ;
#8813 = EDGE_CURVE ( 'NONE', #11175, #9756, #6318, .T. ) ;
#8814 = CARTESIAN_POINT ( 'NONE',  ( 10.40609041963844028, 2.453994274272181197, -106.8025912277847738 ) ) ;
#8815 = CARTESIAN_POINT ( 'NONE',  ( -25.78218315853617781, 8.673617379884035472E-16, -191.6593332018818217 ) ) ;
#8816 = DIRECTION ( 'NONE',  ( 0.000000000000000000, 1.000000000000000000, 0.000000000000000000 ) ) ;
#8817 = DESIGN_CONTEXT ( 'detailed design', #8173, 'design' ) ;
#8818 =( BOUNDED_SURFACE ( )  B_SPLINE_SURFACE ( 3, 2, ( 
 ( #13045, #12112, #10876 ),
 ( #4773, #10960, #3854 ),
 ( #295, #1298, #1530 ),
 ( #8476, #9489, #12976 ),
 ( #2455, #5010, #9727 ),
 ( #2537, #379, #5087 ),
 ( #9801, #14457, #11952 ),
 ( #7152, #14531, #8249 ),
 ( #11874, #2380, #7078 ),
 ( #11798, #4849, #1212 ),
 ( #5922, #9640, #10796 ),
 ( #14213, #210, #9560 ),
 ( #10648, #4923, #13210 ),
 ( #3685, #5999, #3615 ),
 ( #14285, #8394, #14373 ),
 ( #13127, #3772, #2613 ),
 ( #2771, #12340, #10185 ),
 ( #454, #9875, #14767 ),
 ( #7475, #6322, #5316 ),
 ( #13595, #3929, #8628 ) ),
 .UNSPECIFIED., .F., .F., .F. ) 
 B_SPLINE_SURFACE_WITH_KNOTS ( ( 4, 2, 2, 2, 2, 2, 2, 2, 2, 4 ),
 ( 3, 3 ),
 ( -1.605708952745050187E-05, 0.0007915698365215041894, 0.001599196762570458813, 0.002406823688619413436, 0.002810637151643890531, 0.003214450614668368060, 0.004022077540717322250, 0.004829704466766277307, 0.005637331392815232364, 0.006444958318864186554 ),
 ( 0.000000000000000000, 1.000000000000000000 ),
 .UNSPECIFIED. ) 
 GEOMETRIC_REPRESENTATION_ITEM ( )  RATIONAL_B_SPLINE_SURFACE ( (
 ( 1.000000000000000000, 1.000000000000000000, 1.000000000000000000),
 ( 1.000000000000000000, 1.000000004030991319, 1.000000000000000000),
 ( 1.000000000000000000, 0.9993280885290816151, 1.000000000000000000),
 ( 1.000000000000000000, 0.9965616808472221866, 1.000000000000000000),
 ( 1.000000000000000000, 0.9944483308498629492, 1.000000000000000000),
 ( 1.000000000000000000, 0.9887906551701354241, 1.000000000000000000),
 ( 1.000000000000000000, 0.9853034643475333532, 1.000000000000000000),
 ( 1.000000000000000000, 0.9792464072626098082, 1.000000000000000000),
 ( 1.000000000000000000, 0.9770901656133914592, 1.000000000000000000),
 ( 1.000000000000000000, 0.9725405627970424849, 1.000000000000000000),
 ( 1.000000000000000000, 0.9701365459986746043, 1.000000000000000000),
 ( 1.000000000000000000, 0.9628092176376522593, 1.000000000000000000),
 ( 1.000000000000000000, 0.9577259713103128957, 1.000000000000000000),
 ( 1.000000000000000000, 0.9478123764691049891, 1.000000000000000000),
 ( 1.000000000000000000, 0.9429374510257780839, 1.000000000000000000),
 ( 1.000000000000000000, 0.9346631652659601608, 1.000000000000000000),
 ( 1.000000000000000000, 0.9312238446806561099, 1.000000000000000000),
 ( 1.000000000000000000, 0.9264379836092896392, 1.000000000000000000),
 ( 1.000000000000000000, 0.9251151247725492022, 1.000000000000000000),
 ( 1.000000000000000000, 0.9251337988227200659, 1.000000000000000000) ) ) 
 REPRESENTATION_ITEM ( '' )  SURFACE ( )  );
#8819 = CARTESIAN_POINT ( 'NONE',  ( -40.43640613370096304, 15.00000000000000000, -157.5381262016960875 ) ) ;
#8820 = CARTESIAN_POINT ( 'NONE',  ( 0.000000000000000000, 13.50000000000000178, 0.2500000000000002220 ) ) ;
#8821 = ORIENTED_EDGE ( 'NONE', *, *, #12124, .F. ) ;
#8822 = DIRECTION ( 'NONE',  ( -1.000000000000000000, 0.000000000000000000, 0.000000000000000000 ) ) ;
#8823 = DIRECTION ( 'NONE',  ( 1.000000000000000000, 0.000000000000000000, 0.000000000000000000 ) ) ;
#8824 = CARTESIAN_POINT ( 'NONE',  ( -3.750000000000000000, 7.687500000000000000, -1.946699141100893149 ) ) ;
#8825 = CARTESIAN_POINT ( 'NONE',  ( -3.724891368794482904, 9.650666666666662508, -47.87745094654707145 ) ) ;
#8826 = CARTESIAN_POINT ( 'NONE',  ( 3.249999999999999556, 8.250000000000000000, -3.500000000000000000 ) ) ;
#8827 = CARTESIAN_POINT ( 'NONE',  ( 3.749999999999999112, 0.1875000000000000833, -5.053300858899108405 ) ) ;
#8828 = LINE ( 'NONE', #14956, #8161 ) ;
#8829 = DIRECTION ( 'NONE',  ( -0.7575874476598363216, -0.000000000000000000, -0.6527336816407245390 ) ) ;
#8830 = DATE_TIME_ROLE ( 'creation_date' ) ;
#8831 = CARTESIAN_POINT ( 'NONE',  ( 3.249999999999999112, 13.81250000000000000, -2.153805922287439945 ) ) ;
#8832 = CARTESIAN_POINT ( 'NONE',  ( -5.799297919316144245, 10.00000000000000355, -109.6563063839760588 ) ) ;
#8833 = ADVANCED_FACE ( 'NONE', ( #9946 ), #4983, .F. ) ;
#8834 = CARTESIAN_POINT ( 'NONE',  ( -0.3766621274091715987, 0.5000000000000000000, -7.146945437571387671 ) ) ;
#8835 = CARTESIAN_POINT ( 'NONE',  ( 8.592224267316021624, 5.000000000000000888, -111.5170830772279515 ) ) ;
#8836 = CARTESIAN_POINT ( 'NONE',  ( 10.01939027896081491, 0.000000000000000000, -127.6977514918621637 ) ) ;
#8837 = DIRECTION ( 'NONE',  ( 0.000000000000000000, 0.000000000000000000, -1.000000000000000000 ) ) ;
#8838 = ORIENTED_EDGE ( 'NONE', *, *, #14209, .T. ) ;
#8839 = CARTESIAN_POINT ( 'NONE',  ( 8.942896775526056885, 11.26065431988117638, 2.518669333141213773 ) ) ;
#8840 = CARTESIAN_POINT ( 'NONE',  ( 1.624578347342659157, 15.00000000000000178, -110.6108487083152596 ) ) ;
#8841 = CARTESIAN_POINT ( 'NONE',  ( 1.553300858899105963, 0.5625000000000001110, -7.250000000000000888 ) ) ;
#8842 = CARTESIAN_POINT ( 'NONE',  ( 3.249999999999998224, 9.312500000000001776, -2.153805922287439945 ) ) ;
#8843 = CARTESIAN_POINT ( 'NONE',  ( -1.346194077712559389, 0.06250000000000000000, -0.2500000000000002220 ) ) ;
#8844 = EDGE_LOOP ( 'NONE', ( #8914, #3913, #6348, #6802 ) ) ;
#8845 = CARTESIAN_POINT ( 'NONE',  ( -2.298097038856278918, 12.37500000000000000, -5.798097038856277585 ) ) ;
#8846 = PRODUCT_DEFINITION ( 'UNKNOWN', '', #12333, #6498 ) ;
#8847 = CARTESIAN_POINT ( 'NONE',  ( -0.2500000000000000555, 4.500000000000000888, -0.2499999999999997780 ) ) ;
#8848 = DIRECTION ( 'NONE',  ( 0.000000000000000000, -1.000000000000000000, 0.000000000000000000 ) ) ;
#8849 = FACE_OUTER_BOUND ( 'NONE', #2138, .T. ) ;
#8850 = CARTESIAN_POINT ( 'NONE',  ( -5.534063745946611768, 14.90222776335429700, -117.1292924427878575 ) ) ;
#8851 = SECURITY_CLASSIFICATION_LEVEL ( 'unclassified' ) ;
#8852 = EDGE_CURVE ( 'NONE', #14170, #14051, #6738, .T. ) ;
#8853 = CARTESIAN_POINT ( 'NONE',  ( 9.875992363739401370, 12.49999999999999822, -120.1725736630937007 ) ) ;
#8854 = ADVANCED_FACE ( 'NONE', ( #7618 ), #13167, .F. ) ;
#8855 = EDGE_CURVE ( 'NONE', #13498, #973, #289, .T. ) ;
#8856 = ORIENTED_EDGE ( 'NONE', *, *, #4054, .T. ) ;
#8857 = CARTESIAN_POINT ( 'NONE',  ( 2.298097038856279362, 3.875000000000000000, -1.201902961143720860 ) ) ;
#8858 = DIRECTION ( 'NONE',  ( 0.000000000000000000, 1.000000000000000000, 0.000000000000000000 ) ) ;
#8859 = CARTESIAN_POINT ( 'NONE',  ( -4.592425496802573972E-16, 14.50000000000000000, -7.249999999999999112 ) ) ;
#8860 = ORIENTED_EDGE ( 'NONE', *, *, #839, .T. ) ;
#8861 = CC_DESIGN_DATE_AND_TIME_ASSIGNMENT ( #4130, #8830, ( #10001 ) ) ;
#8862 = CARTESIAN_POINT ( 'NONE',  ( 51.62524086895221842, 0.000000000000000000, 69.88209797381232136 ) ) ;
#8863 = CARTESIAN_POINT ( 'NONE',  ( 0.000000000000000000, 2.000000000000000000, 0.2500000000000002220 ) ) ;
#8864 = CARTESIAN_POINT ( 'NONE',  ( 7.349173144666838020, 3.814570804032795692, -25.35250733039552884 ) ) ;
#8865 = CARTESIAN_POINT ( 'NONE',  ( 0.3189473520463899647, 0.8338976723007026637, 3.612722554896655947 ) ) ;
#8866 = CARTESIAN_POINT ( 'NONE',  ( 0.000000000000000000, 1.000000000000000000, 0.2500000000000002220 ) ) ;
#8867 = APPROVAL_DATE_TIME ( #10030, #2516 ) ;
#8868 = PLANE ( 'NONE',  #98 ) ;
#8869 = CYLINDRICAL_SURFACE ( 'NONE', #4466, 3.500000000000000000 ) ;
#8870 = EDGE_CURVE ( 'NONE', #8603, #6034, #3524, .T. ) ;
#8871 = ORIENTED_EDGE ( 'NONE', *, *, #7256, .T. ) ;
#8872 = PRODUCT_DEFINITION ( 'UNKNOWN', '', #11824, #12369 ) ;
#8873 = CARTESIAN_POINT ( 'NONE',  ( -0.3766621274091715987, 0.2398196381212478467, -0.1347136637304948426 ) ) ;
#8874 = CARTESIAN_POINT ( 'NONE',  ( -3.249999999999999112, 2.687500000000000888, -2.153805922287440833 ) ) ;
#8875 = CARTESIAN_POINT ( 'NONE',  ( -2.298097038856279362, 11.87500000000000000, -5.798097038856278473 ) ) ;
#8876 = DIRECTION ( 'NONE',  ( -0.1564344650402312298, -0.000000000000000000, 0.9876883405951376593 ) ) ;
#8877 = DIRECTION ( 'NONE',  ( 0.08794243244722413366, 0.000000000000000000, 0.9961255586397056438 ) ) ;
#8878 = CARTESIAN_POINT ( 'NONE',  ( 2.298097038856279362, 2.875000000000000000, -1.201902961143720860 ) ) ;
#8879 = CARTESIAN_POINT ( 'NONE',  ( 3.749999999999999556, 6.250000000000000000, -3.500000000000000444 ) ) ;
#8880 = CARTESIAN_POINT ( 'NONE',  ( -3.750000000000000000, 8.312500000000000000, -5.053300858899105741 ) ) ;
#8881 = LOCAL_TIME ( 12, 28, 20.00000000000000000, #1440 ) ;
#8882 = CARTESIAN_POINT ( 'NONE',  ( -4.887975900231388060, 0.02948499366869817423, -117.2415000213202774 ) ) ;
#8883 = ORIENTED_EDGE ( 'NONE', *, *, #935, .T. ) ;
#8884 = LINE ( 'NONE', #2938, #1259 ) ;
#8885 = CARTESIAN_POINT ( 'NONE',  ( -2.651650429449552870, 11.62500000000000000, -0.8483495705504463524 ) ) ;
#8886 = CARTESIAN_POINT ( 'NONE',  ( 4.052988422354451004, 9.999999999999998224, -106.4147896264523467 ) ) ;
#8887 = CIRCLE ( 'NONE', #754, 2.000000000000007994 ) ;
#8888 = CARTESIAN_POINT ( 'NONE',  ( 6.577825583858426306, 0.000000000000000000, -139.0000488628143103 ) ) ;
#8889 = CARTESIAN_POINT ( 'NONE',  ( 38.72419741971091867, 2.100000000000000089, 40.93614862128714549 ) ) ;
#8890 = CARTESIAN_POINT ( 'NONE',  ( -23.30526566008802902, 8.673617379884035472E-16, -178.8465041759440055 ) ) ;
#8891 = DIRECTION ( 'NONE',  ( 0.000000000000000000, 0.000000000000000000, 1.000000000000000000 ) ) ;
#8892 = CARTESIAN_POINT ( 'NONE',  ( -45.52432922698630335, 15.00000000000539480, -160.5926188986776992 ) ) ;
#8893 = LOCAL_TIME ( 12, 28, 20.00000000000000000, #1422 ) ;
#8894 = CARTESIAN_POINT ( 'NONE',  ( -1.346194077712558945, -0.4374999999999998890, -0.2500000000000002220 ) ) ;
#8895 = VERTEX_POINT ( 'NONE', #8862 ) ;
#8896 = FACE_OUTER_BOUND ( 'NONE', #5616, .T. ) ;
#8897 = DIRECTION ( 'NONE',  ( 0.000000000000000000, 0.000000000000000000, 1.000000000000000000 ) ) ;
#8898 = CARTESIAN_POINT ( 'NONE',  ( -1.553300858899106629, 10.56250000000000355, 0.2499999999999998335 ) ) ;
#8899 = AXIS2_PLACEMENT_3D ( 'NONE', #4199, #12463, #14571 ) ;
#8900 = CARTESIAN_POINT ( 'NONE',  ( -3.345593546076259361, 10.60898574532662941, -45.14660385735189152 ) ) ;
#8901 = CARTESIAN_POINT ( 'NONE',  ( -3.249999999999999556, 6.750000000000000888, -3.500000000000000000 ) ) ;
#8902 = CARTESIAN_POINT ( 'NONE',  ( -32.48742309669081862, 9.999999999999998224, -156.1716796081720133 ) ) ;
#8903 = CARTESIAN_POINT ( 'NONE',  ( 2.651650429449553759, 11.87500000000000000, -0.8483495705504471296 ) ) ;
#8904 = CARTESIAN_POINT ( 'NONE',  ( -68.19209817482972369, 15.00000000000174438, -203.2686135464926451 ) ) ;
#8905 = CIRCLE ( 'NONE', #6184, 3.750000000000003109 ) ;
#8906 = CARTESIAN_POINT ( 'NONE',  ( 0.9234955565201180550, -1.734723475976807094E-15, -138.4305453062657421 ) ) ;
#8907 = CARTESIAN_POINT ( 'NONE',  ( -2.298097038856278473, 13.12500000000000000, -1.201902961143720416 ) ) ;
#8908 = CIRCLE ( 'NONE', #3975, 6.999999999999950262 ) ;
#8909 = DIRECTION ( 'NONE',  ( -0.000000000000000000, 1.000000000000000000, -0.000000000000000000 ) ) ;
#8910 = LINE ( 'NONE', #3040, #4083 ) ;
#8911 = CARTESIAN_POINT ( 'NONE',  ( 3.249999999999999112, 6.812500000000000000, -2.153805922287439945 ) ) ;
#8912 = CARTESIAN_POINT ( 'NONE',  ( 3.230086961373113130, 5.000000000000000888, 5.208283729180105404 ) ) ;
#8913 = CARTESIAN_POINT ( 'NONE',  ( 10.99170155471432686, 11.63675136861741244, -45.52739065948508568 ) ) ;
#8914 = ORIENTED_EDGE ( 'NONE', *, *, #11404, .F. ) ;
#8915 = CARTESIAN_POINT ( 'NONE',  ( 7.786518181264857397, 5.211846493442710226, -20.40551834929134856 ) ) ;
#8916 = CARTESIAN_POINT ( 'NONE',  ( -20.28323750239604806, 4.000000000000000000, -200.3886341823752844 ) ) ;
#8917 = CARTESIAN_POINT ( 'NONE',  ( 2.651650429449553759, 0.8750000000000000000, -0.8483495705504471296 ) ) ;
#8918 = CARTESIAN_POINT ( 'NONE',  ( 3.249999999999999556, 10.25000000000000178, -3.500000000000000000 ) ) ;
#8919 = CARTESIAN_POINT ( 'NONE',  ( -2.298097038856278473, 0.1250000000000000000, -1.201902961143720416 ) ) ;
#8920 = VERTEX_POINT ( 'NONE', #13588 ) ;
#8921 = CIRCLE ( 'NONE', #3484, 5.000000000000000000 ) ;
#8922 = CARTESIAN_POINT ( 'NONE',  ( -3.249999999999999556, 11.31249999999999822, -4.846194077712557835 ) ) ;
#8923 = EDGE_CURVE ( 'NONE', #14015, #2518, #12661, .T. ) ;
#8924 = CARTESIAN_POINT ( 'NONE',  ( 10.02810328368141768, 11.68469885172349798, -45.38224167655878460 ) ) ;
#8925 = CARTESIAN_POINT ( 'NONE',  ( 9.945392800007761380, 12.56622419557329096, -43.41640182928829006 ) ) ;
#8926 = CARTESIAN_POINT ( 'NONE',  ( 5.595249735037589822, 2.348479801108206200, 4.434930130517638069 ) ) ;
#8927 = CARTESIAN_POINT ( 'NONE',  ( -8.888107754931663607, 12.67556477985378116, -116.5586263778010903 ) ) ;
#8928 = PERSON_AND_ORGANIZATION ( #3176, #3020 ) ;
#8929 = VECTOR ( 'NONE', #3302, 1000.000000000000000 ) ;
#8930 = CARTESIAN_POINT ( 'NONE',  ( 9.218878510548623950, 15.00000000000000000, -124.0543039030355601 ) ) ;
#8931 = APPROVAL ( #6245, 'UNSPECIFIED' ) ;
#8932 = CARTESIAN_POINT ( 'NONE',  ( 27.11959404819519293, 3.246087323616470233, -137.4897650963793296 ) ) ;
#8933 = VERTEX_POINT ( 'NONE', #5004 ) ;
#8934 = CARTESIAN_POINT ( 'NONE',  ( -2.298097038856278473, 3.125000000000000000, -1.201902961143720416 ) ) ;
#8935 = CARTESIAN_POINT ( 'NONE',  ( -22.38716924508033657, 4.000000000000000000, -164.7809911966533889 ) ) ;
#8936 = CARTESIAN_POINT ( 'NONE',  ( -3.749999999999999556, 2.750000000000000444, -3.499999999999999112 ) ) ;
#8937 = ORIENTED_EDGE ( 'NONE', *, *, #1292, .F. ) ;
#8938 = DIRECTION ( 'NONE',  ( -0.9961255586397050887, -0.000000000000000000, 0.08794243244723005948 ) ) ;
#8939 = PRODUCT_DEFINITION_FORMATION_WITH_SPECIFIED_SOURCE ( 'ANY', '', #3617, .NOT_KNOWN. ) ;
#8940 = CARTESIAN_POINT ( 'NONE',  ( 1.553300858899105963, 0.5625000000000001110, -7.250000000000000888 ) ) ;
#8941 = EDGE_CURVE ( 'NONE', #8920, #1352, #2545, .T. ) ;
#8942 = CARTESIAN_POINT ( 'NONE',  ( -60.91137729732987793, 5.000000000000000888, -175.0198515626273661 ) ) ;
#8943 = CARTESIAN_POINT ( 'NONE',  ( 2.803776756569541284, 0.2483257210975995111, 1.809827704450910568 ) ) ;
#8944 = CARTESIAN_POINT ( 'NONE',  ( 3.749999999999999556, 1.812500000000000000, -1.946699141100892261 ) ) ;
#8945 = COORDINATED_UNIVERSAL_TIME_OFFSET ( 0, 0, .AHEAD. ) ;
#8946 = CARTESIAN_POINT ( 'NONE',  ( 13.52340959288768651, 5.000000000000000888, -125.7424794682274438 ) ) ;
#8947 = CARTESIAN_POINT ( 'NONE',  ( 0.000000000000000000, 5.000000000000000000, 0.000000000000000000 ) ) ;
#8948 = ORIENTED_EDGE ( 'NONE', *, *, #2913, .T. ) ;
#8949 = CARTESIAN_POINT ( 'NONE',  ( 8.990769910733003911, 12.49999999999999822, 0.3250886916252374026 ) ) ;
#8950 = CARTESIAN_POINT ( 'NONE',  ( 1.346194077712558279, 2.062500000000000000, -6.750000000000000888 ) ) ;
#8951 = DIRECTION ( 'NONE',  ( -0.000000000000000000, 1.000000000000000000, -0.000000000000000000 ) ) ;
#8952 = LINE ( 'NONE', #1773, #11688 ) ;
#8953 = CARTESIAN_POINT ( 'NONE',  ( -3.749999999999999556, 4.750000000000000000, -3.499999999999999112 ) ) ;
#8954 = EDGE_CURVE ( 'NONE', #2235, #10316, #3842, .T. ) ;
#8955 = CARTESIAN_POINT ( 'NONE',  ( -4.592425496802573972E-16, 9.500000000000000000, -7.249999999999999112 ) ) ;
#8956 = CARTESIAN_POINT ( 'NONE',  ( -4.561986575600236016, 1.189234257945038070E-15, -117.3660065143490812 ) ) ;
#8957 = CARTESIAN_POINT ( 'NONE',  ( -5.928758847211441640, 0.2324570288725731071, -117.1828119328369695 ) ) ;
#8958 = CARTESIAN_POINT ( 'NONE',  ( -1.346194077712559389, 8.062500000000000000, -0.2500000000000002220 ) ) ;
#8959 = CARTESIAN_POINT ( 'NONE',  ( 1.553300858899105963, 9.062500000000000000, -7.250000000000000888 ) ) ;
#8960 = CARTESIAN_POINT ( 'NONE',  ( -1.500000000000000000, 5.000000000000000000, -0.2499999999999997780 ) ) ;
#8961 = DIRECTION ( 'NONE',  ( 0.000000000000000000, 0.000000000000000000, 1.000000000000000000 ) ) ;
#8962 = CIRCLE ( 'NONE', #2303, 5.000000000000000000 ) ;
#8963 = CARTESIAN_POINT ( 'NONE',  ( 3.358120751865298903, 2.099999999996547295, 2.798954194608255897 ) ) ;
#8964 = VERTEX_POINT ( 'NONE', #6623 ) ;
#8965 = CARTESIAN_POINT ( 'NONE',  ( -13.94227320128385017, 1.734723475976807094E-15, -160.5206178152066343 ) ) ;
#8966 = CARTESIAN_POINT ( 'NONE',  ( -14.68073284315481253, 7.499999999999991118, -92.37694453701993780 ) ) ;
#8967 = CARTESIAN_POINT ( 'NONE',  ( -29.69515346086419072, 9.999999999999998224, -156.7390981038714983 ) ) ;
#8968 = CARTESIAN_POINT ( 'NONE',  ( 3.249999999999998224, 2.312500000000000000, -2.153805922287439945 ) ) ;
#8969 = EDGE_LOOP ( 'NONE', ( #11518, #9617, #15280, #8143 ) ) ;
#8970 = DIRECTION ( 'NONE',  ( -0.000000000000000000, -1.000000000000000000, -0.000000000000000000 ) ) ;
#8971 = FACE_OUTER_BOUND ( 'NONE', #8253, .T. ) ;
#8972 =( REPRESENTATION_RELATIONSHIP ('NONE','NONE', #11394, #7636 ) REPRESENTATION_RELATIONSHIP_WITH_TRANSFORMATION ( #10019 )SHAPE_REPRESENTATION_RELATIONSHIP( ) );
#8973 = CARTESIAN_POINT ( 'NONE',  ( -3.332125856844564638, 10.29293441821257282, -44.11502059987310531 ) ) ;
#8974 = CARTESIAN_POINT ( 'NONE',  ( 0.000000000000000000, 5.000000000000000000, 0.000000000000000000 ) ) ;
#8975 = CARTESIAN_POINT ( 'NONE',  ( -3.768042520877054269, 1.734723475976807094E-15, -109.5986228335332129 ) ) ;
#8976 = CIRCLE ( 'NONE', #8218, 5.000000000000000000 ) ;
#8977 = CARTESIAN_POINT ( 'NONE',  ( 2.298097038856278029, 9.125000000000001776, -5.798097038856279362 ) ) ;
#8978 = AXIS2_PLACEMENT_3D ( 'NONE', #13808, #12565, #11554 ) ;
#8979 = DIRECTION ( 'NONE',  ( 0.000000000000000000, -1.000000000000000000, 0.000000000000000000 ) ) ;
#8980 = CARTESIAN_POINT ( 'NONE',  ( 3.749999999999998668, 14.68750000000000000, -5.053300858899107517 ) ) ;
#8981 = DIRECTION ( 'NONE',  ( -0.08794243244722413366, 0.000000000000000000, -0.9961255586397056438 ) ) ;
#8982 = DIRECTION ( 'NONE',  ( 0.000000000000000000, 1.000000000000000000, 0.000000000000000000 ) ) ;
#8983 = CARTESIAN_POINT ( 'NONE',  ( -3.249999999999999556, 11.25000000000000000, -3.499999999999999556 ) ) ;
#8984 = CARTESIAN_POINT ( 'NONE',  ( 6.369258321017759350, 2.075239479414269894, -34.56909192082981974 ) ) ;
#8985 = LINE ( 'NONE', #4425, #372 ) ;
#8986 = CARTESIAN_POINT ( 'NONE',  ( -2.298097038856278473, 10.12500000000000000, -1.201902961143720416 ) ) ;
#8987 = AXIS2_PLACEMENT_3D ( 'NONE', #2469, #6014, #3628 ) ;
#8988 = CARTESIAN_POINT ( 'NONE',  ( 10.01939027896081669, 5.000000000000000888, -127.6977514918621637 ) ) ;
#8989 = CARTESIAN_POINT ( 'NONE',  ( -9.721966606378851239, 5.000000000000000888, -116.3614657639809309 ) ) ;
#8990 = EDGE_LOOP ( 'NONE', ( #4376, #12873, #15285, #10534 ) ) ;
#8991 = CARTESIAN_POINT ( 'NONE',  ( 8.954409718278865782, 11.89299648869835835, 1.991138219077579041 ) ) ;
#8992 = CARTESIAN_POINT ( 'NONE',  ( 12.76858567064540217, 3.999999999993260502, -166.6103056774037441 ) ) ;
#8993 = CARTESIAN_POINT ( 'NONE',  ( -1.553300858899107295, 1.437500000000000000, -7.250000000000000000 ) ) ;
#8994 = CARTESIAN_POINT ( 'NONE',  ( -1.346194077712558945, 14.56250000000000000, -0.2500000000000002220 ) ) ;
#8995 = CARTESIAN_POINT ( 'NONE',  ( 3.249999999999999556, 13.25000000000000000, -3.500000000000000000 ) ) ;
#8996 = VERTEX_POINT ( 'NONE', #3067 ) ;
#8997 = CARTESIAN_POINT ( 'NONE',  ( 3.249999999999999112, 10.81250000000000178, -2.153805922287439945 ) ) ;
#8998 = VECTOR ( 'NONE', #11302, 1000.000000000000114 ) ;
#8999 = DIRECTION ( 'NONE',  ( -0.000000000000000000, 0.000000000000000000, 1.000000000000000000 ) ) ;
#9000 = CARTESIAN_POINT ( 'NONE',  ( -7.885911378209643274, 13.39228090171942931, -104.2457333304612206 ) ) ;
#9001 = CARTESIAN_POINT ( 'NONE',  ( -4.018470066652908734, 7.379999999999995453, -45.51728475810764962 ) ) ;
#9002 = CARTESIAN_POINT ( 'NONE',  ( -25.82983890416511841, 15.00000000000000000, -142.4527639562402328 ) ) ;
#9003 = APPROVAL_STATUS ( 'not_yet_approved' ) ;
#9004 = EDGE_CURVE ( 'NONE', #14341, #13571, #6607, .T. ) ;
#9005 = CARTESIAN_POINT ( 'NONE',  ( 11.07647859176971039, 15.00000000000000000, -126.6612394307274911 ) ) ;
#9006 = DIRECTION ( 'NONE',  ( -0.000000000000000000, 1.000000000000000000, -0.000000000000000000 ) ) ;
#9007 = CARTESIAN_POINT ( 'NONE',  ( 23.17896007687009075, 0.3998921152608300722, -138.1654099684218409 ) ) ;
#9008 = ORIENTED_EDGE ( 'NONE', *, *, #6202, .F. ) ;
#9009 = EDGE_CURVE ( 'NONE', #698, #5136, #13811, .T. ) ;
#9010 = CARTESIAN_POINT ( 'NONE',  ( -3.249999999999999556, 6.187500000000000888, -2.153805922287440833 ) ) ;
#9011 = CARTESIAN_POINT ( 'NONE',  ( -17.32624372123753886, 2.500000000000000444, -122.3796757791585321 ) ) ;
#9012 = CARTESIAN_POINT ( 'NONE',  ( 2.651650429449552870, 0.1250000000000001110, -6.151650429449555091 ) ) ;
#9013 = ORIENTED_EDGE ( 'NONE', *, *, #7717, .F. ) ;
#9014 = B_SPLINE_CURVE_WITH_KNOTS ( 'NONE', 3,
 ( #4393, #11570, #14928, #10418, #5397, #7941, #4324, #9028, #12815, #8089, #2222, #6711, #10112, #5548, #13910, #12504 ),
 .UNSPECIFIED., .F., .F.,
 ( 4, 2, 2, 2, 2, 2, 2, 4 ),
 ( 3.469446951953614189E-18, 0.0005010218446280251129, 0.001002043689256046756, 0.001503065533884068291, 0.002004087378512090043, 0.002505109223140111578, 0.003006131067768133113, 0.004008174757024192229 ),
 .UNSPECIFIED. ) ;
#9015 = CARTESIAN_POINT ( 'NONE',  ( -6.738069272571859614, 14.39261927056258372, -116.5044176451309852 ) ) ;
#9016 = DIRECTION ( 'NONE',  ( 0.08794243244722425856, 0.000000000000000000, 0.9961255586397054218 ) ) ;
#9017 = CARTESIAN_POINT ( 'NONE',  ( -2.651650429449553314, 7.375000000000000888, -6.151650429449552426 ) ) ;
#9018 = CARTESIAN_POINT ( 'NONE',  ( -33.91109452335874153, 10.00000000000000178, -156.1716796081737471 ) ) ;
#9019 = CARTESIAN_POINT ( 'NONE',  ( -47.48189921986828210, 15.00000000000000000, -141.5723758807981483 ) ) ;
#9020 = CARTESIAN_POINT ( 'NONE',  ( 0.000000000000000000, 3.000000000000000000, 0.2500000000000002220 ) ) ;
#9021 = APPROVAL_STATUS ( 'not_yet_approved' ) ;
#9022 = CARTESIAN_POINT ( 'NONE',  ( 24.07280085736360675, 5.000000000000000888, -135.1358744081167913 ) ) ;
#9023 = PLANE ( 'NONE',  #8397 ) ;
#9024 = VERTEX_POINT ( 'NONE', #7930 ) ;
#9025 = EDGE_CURVE ( 'NONE', #12332, #15113, #10099, .T. ) ;
#9026 = CARTESIAN_POINT ( 'NONE',  ( -0.1258718175769854841, 0.2162433659573944622, -0.1347136637304948981 ) ) ;
#9027 = CARTESIAN_POINT ( 'NONE',  ( -1.346194077712559167, 4.937500000000000000, -6.749999999999999112 ) ) ;
#9028 = CARTESIAN_POINT ( 'NONE',  ( 10.58382518318612320, 14.03954883485831751, -106.8470192801346030 ) ) ;
#9029 = CARTESIAN_POINT ( 'NONE',  ( -9.302736714094232084, 2.500000000000000444, -123.7731201992051098 ) ) ;
#9030 = CARTESIAN_POINT ( 'NONE',  ( 3.749999999999999112, 8.312500000000003553, -1.946699141100893149 ) ) ;
#9031 = CARTESIAN_POINT ( 'NONE',  ( -4.592425496802573972E-16, 12.50000000000000000, -7.249999999999999112 ) ) ;
#9032 = CARTESIAN_POINT ( 'NONE',  ( -4.234402844927150689, 0.000000000000000000, -117.4888040839639558 ) ) ;
#9033 = ORIENTED_EDGE ( 'NONE', *, *, #4363, .F. ) ;
#9034 = CARTESIAN_POINT ( 'NONE',  ( -9.721966606378851239, 5.000000000000000888, -116.3614657639809309 ) ) ;
#9035 = CARTESIAN_POINT ( 'NONE',  ( 0.000000000000000000, 8.000000000000000000, -0.2500000000000002220 ) ) ;
#9036 = CARTESIAN_POINT ( 'NONE',  ( -1.553300858899107073, 8.937500000000000000, -7.249999999999999112 ) ) ;
#9037 = CARTESIAN_POINT ( 'NONE',  ( -5.054995719515170904, 4.336808689942017736E-16, -105.8433260022760294 ) ) ;
#9038 = CC_DESIGN_DATE_AND_TIME_ASSIGNMENT ( #5524, #5232, ( #4203 ) ) ;
#9039 = CARTESIAN_POINT ( 'NONE',  ( 8.236624398825258098, 15.00000000000000000, -106.5667377758158523 ) ) ;
#9040 = FACE_OUTER_BOUND ( 'NONE', #2718, .T. ) ;
#9041 = ORIENTED_EDGE ( 'NONE', *, *, #12833, .T. ) ;
#9042 = ADVANCED_FACE ( 'NONE', ( #6774 ), #11913, .T. ) ;
#9043 = CARTESIAN_POINT ( 'NONE',  ( -28.70971482902378114, 3.999999999999513278, -179.7031761687850349 ) ) ;
#9044 = CARTESIAN_POINT ( 'NONE',  ( 11.77099615976924163, 1.493628967302184973, -165.6844967162601279 ) ) ;
#9045 = ADVANCED_FACE ( 'NONE', ( #4234 ), #11490, .F. ) ;
#9046 = CARTESIAN_POINT ( 'NONE',  ( -48.42971706878667959, 9.999999999999998224, -163.2864622073098246 ) ) ;
#9047 = ADVANCED_FACE ( 'NONE', ( #2139 ), #7728, .T. ) ;
#9048 = CARTESIAN_POINT ( 'NONE',  ( -3.980102097228897738E-16, 4.000000000000000888, -6.749999999999999112 ) ) ;
#9049 = ORIENTED_EDGE ( 'NONE', *, *, #2836, .T. ) ;
#9050 = DIRECTION ( 'NONE',  ( -0.000000000000000000, 1.000000000000000000, 0.000000000000000000 ) ) ;
#9051 = CARTESIAN_POINT ( 'NONE',  ( 2.678407845566781020, -1.921202954650395700, -1.000000000000023537 ) ) ;
#9052 = CARTESIAN_POINT ( 'NONE',  ( -25.14123021401396940, 8.651900396264618934E-15, -199.0874206847575749 ) ) ;
#9053 = CARTESIAN_POINT ( 'NONE',  ( 6.410864412206024987, 14.96873749810645826, 0.9153280175020522824 ) ) ;
#9054 = CARTESIAN_POINT ( 'NONE',  ( 4.246495378557483491, 8.673617379884035472E-16, -105.2373590921493758 ) ) ;
#9055 = CARTESIAN_POINT ( 'NONE',  ( 2.298097038856278029, 10.12500000000000000, -5.798097038856279362 ) ) ;
#9056 = CARTESIAN_POINT ( 'NONE',  ( 24.53888684075532467, 2.337595819977410685E-12, -142.6514391812058591 ) ) ;
#9057 = CARTESIAN_POINT ( 'NONE',  ( 2.651650429449552870, 13.62500000000000000, -6.151650429449554203 ) ) ;
#9058 = DIRECTION ( 'NONE',  ( 0.08794243244723000397, 0.000000000000000000, 0.9961255586397049777 ) ) ;
#9059 = CARTESIAN_POINT ( 'NONE',  ( 17.50071171097425804, 8.749999999999998224, -91.70093451412481045 ) ) ;
#9060 = CARTESIAN_POINT ( 'NONE',  ( 1.346194077712560944, 13.93750000000000000, -0.2500000000000010547 ) ) ;
#9061 = CARTESIAN_POINT ( 'NONE',  ( -0.6421131273608506884, 2.743867526398027223, -43.87268297926053151 ) ) ;
#9062 = CARTESIAN_POINT ( 'NONE',  ( 4.798865512804554534, 14.61883240900064607, 1.001995710397592498 ) ) ;
#9063 = CARTESIAN_POINT ( 'NONE',  ( 2.298097038856279362, 7.875000000000000000, -1.201902961143720860 ) ) ;
#9064 = CARTESIAN_POINT ( 'NONE',  ( 10.01939027896081313, 9.999999999999998224, -127.6977514918621637 ) ) ;
#9065 = CARTESIAN_POINT ( 'NONE',  ( -8.886921396801799489, 2.500000000000000444, -105.5168766094550250 ) ) ;
#9066 = ORIENTED_EDGE ( 'NONE', *, *, #12215, .T. ) ;
#9067 = CARTESIAN_POINT ( 'NONE',  ( 9.980434402550784512, 5.834507182123311431, -43.94877651782068995 ) ) ;
#9068 = B_SPLINE_CURVE_WITH_KNOTS ( 'NONE', 3,
 ( #11247, #5374, #819, #14673, #14822, #12557, #13510, #10016, #11398, #4221 ),
 .UNSPECIFIED., .F., .F.,
 ( 4, 2, 2, 2, 4 ),
 ( 0.000000000000000000, 0.0002464242564425689190, 0.0004928485128851378379, 0.0007392727693277068111, 0.0009856970257702756758 ),
 .UNSPECIFIED. ) ;
#9069 = CARTESIAN_POINT ( 'NONE',  ( 8.571367539318496043, 12.50000000000000000, -116.3909463212235806 ) ) ;
#9070 = CARTESIAN_POINT ( 'NONE',  ( 2.651650429449552870, 0.6250000000000000000, -6.151650429449554203 ) ) ;
#9071 = CARTESIAN_POINT ( 'NONE',  ( 2.298097038856279362, 13.37500000000000000, -1.201902961143720860 ) ) ;
#9072 = CARTESIAN_POINT ( 'NONE',  ( 1.346194077712558057, 0.5625000000000001110, -6.750000000000000000 ) ) ;
#9073 = ORIENTED_EDGE ( 'NONE', *, *, #13279, .F. ) ;
#9074 = B_SPLINE_CURVE_WITH_KNOTS ( 'NONE', 3,
 ( #5012, #12115, #8715, #13289, #5244, #7392, #381, #10962, #13526, #9953, #4093, #2924, #1612, #1452, #13450, #4013, #2773, #6324, #1684, #2855, #13600, #7555, #12274, #7477, #456, #1533 ),
 .UNSPECIFIED., .F., .F.,
 ( 4, 2, 2, 2, 2, 2, 2, 2, 2, 2, 2, 2, 4 ),
 ( -8.569047602456792291E-05, 0.006541394408673478593, 0.009854936851022505842, 0.01316847929337153396, 0.01648202173572056381, 0.01979556417806959193, 0.02145233539924410598, 0.02310910662041862351, 0.02393749223100587881, 0.02476587784159313757, 0.02559426345218039980, 0.02600845625747404133, 0.02642264906276768632 ),
 .UNSPECIFIED. ) ;
#9075 = CARTESIAN_POINT ( 'NONE',  ( -3.980102097228897245E-16, 12.50000000000000000, -6.749999999999999112 ) ) ;
#9076 = DIRECTION ( 'NONE',  ( 1.000000000000000000, 0.000000000000000000, 0.000000000000000000 ) ) ;
#9077 = CARTESIAN_POINT ( 'NONE',  ( -7.841189678847138467, 13.47270973785375148, -104.5808338560114663 ) ) ;
#9078 = CARTESIAN_POINT ( 'NONE',  ( -8.208951728224976208, 13.46737988720133750, -116.7121244410452334 ) ) ;
#9079 = PERSON_AND_ORGANIZATION_ROLE ( 'classification_officer' ) ;
#9080 = CARTESIAN_POINT ( 'NONE',  ( 8.852045268163109881, 12.49999999999999822, -117.5747611282338596 ) ) ;
#9081 = CARTESIAN_POINT ( 'NONE',  ( -9.721966606378851239, 10.00000000000000000, -116.3614657639809309 ) ) ;
#9082 = ORIENTED_EDGE ( 'NONE', *, *, #6102, .F. ) ;
#9083 = CARTESIAN_POINT ( 'NONE',  ( 25.53732853817565740, 1.428021340339478584, -137.8769250524031804 ) ) ;
#9084 = CARTESIAN_POINT ( 'NONE',  ( 3.249999999999999112, 11.81250000000000000, -2.153805922287439945 ) ) ;
#9085 = ORIENTED_EDGE ( 'NONE', *, *, #219, .F. ) ;
#9086 = CARTESIAN_POINT ( 'NONE',  ( -3.980102097228897245E-16, 5.500000000000000000, -6.749999999999999112 ) ) ;
#9087 = CARTESIAN_POINT ( 'NONE',  ( -4.452859729112454978, 4.000000000000000888, -143.4037473448349829 ) ) ;
#9088 = CARTESIAN_POINT ( 'NONE',  ( -3.749999999999999556, 0.7500000000000001110, -3.499999999999999112 ) ) ;
#9089 = ORIENTED_EDGE ( 'NONE', *, *, #4243, .T. ) ;
#9090 = CARTESIAN_POINT ( 'NONE',  ( -7.289398910521209807, 14.05303354678142824, -116.2745874757426918 ) ) ;
#9091 = DIRECTION ( 'NONE',  ( 0.000000000000000000, 0.000000000000000000, 1.000000000000000000 ) ) ;
#9092 = CARTESIAN_POINT ( 'NONE',  ( 3.749999999999999112, 6.812500000000000000, -1.946699141100892039 ) ) ;
#9093 = CARTESIAN_POINT ( 'NONE',  ( -25.32353976185253330, 1.355199924532299205, -206.8830429655051830 ) ) ;
#9094 = CARTESIAN_POINT ( 'NONE',  ( 0.4903027347542082137, 3.623355825888509241, 5.553668143684391545 ) ) ;
#9095 = CALENDAR_DATE ( 2026, 8, 10 ) ;
#9096 = CARTESIAN_POINT ( 'NONE',  ( 11.04730217088350663, 5.000000000000000888, -107.1178495010082941 ) ) ;
#9097 = PLANE ( 'NONE',  #9643 ) ;
#9098 = EDGE_LOOP ( 'NONE', ( #13921, #14829, #1407, #12622, #2747 ) ) ;
#9099 = CARTESIAN_POINT ( 'NONE',  ( 2.298097038856278029, 2.125000000000000000, -5.798097038856279362 ) ) ;
#9100 = FACE_OUTER_BOUND ( 'NONE', #5842, .T. ) ;
#9101 = AXIS2_PLACEMENT_3D ( 'NONE', #8418, #12137, #3710 ) ;
#9102 = ADVANCED_FACE ( 'NONE', ( #13739 ), #5017, .T. ) ;
#9103 = CARTESIAN_POINT ( 'NONE',  ( 3.749999999999998668, 11.18750000000000178, -5.053300858899108405 ) ) ;
#9104 = CARTESIAN_POINT ( 'NONE',  ( -1.553300858899106407, 14.06250000000000178, 0.2500000000000002220 ) ) ;
#9105 = EDGE_CURVE ( 'NONE', #5472, #4732, #8962, .T. ) ;
#9106 = CARTESIAN_POINT ( 'NONE',  ( -64.15738946500745499, 15.00000000058060934, -182.2117518801574931 ) ) ;
#9107 = CARTESIAN_POINT ( 'NONE',  ( -8.265142125449676413, 1.586851510356210415, -116.6996609440855934 ) ) ;
#9108 = CARTESIAN_POINT ( 'NONE',  ( -3.980102097228897738E-16, 1.000000000000000000, -6.749999999999999112 ) ) ;
#9109 = CARTESIAN_POINT ( 'NONE',  ( 11.32016196459919755, 12.66760504685707822, -106.4092894470422124 ) ) ;
#9110 = CARTESIAN_POINT ( 'NONE',  ( 0.000000000000000000, 1.000000000000000000, 0.000000000000000000 ) ) ;
#9111 = EDGE_LOOP ( 'NONE', ( #3574, #4901, #7604, #2323 ) ) ;
#9112 = CARTESIAN_POINT ( 'NONE',  ( -24.40461474964762090, 2.124593680485182396E-15, -208.9486585025150873 ) ) ;
#9113 = CARTESIAN_POINT ( 'NONE',  ( 7.148068729939690336, -2.490287375297125294, -34.56909192082981974 ) ) ;
#9114 = CARTESIAN_POINT ( 'NONE',  ( -42.75031104224877510, 15.00000000000000000, -153.0915108332807790 ) ) ;
#9115 = CARTESIAN_POINT ( 'NONE',  ( -3.249999999999999556, 4.750000000000000888, -3.500000000000000000 ) ) ;
#9116 = ORIENTED_EDGE ( 'NONE', *, *, #13203, .T. ) ;
#9117 = FACE_OUTER_BOUND ( 'NONE', #2264, .T. ) ;
#9118 = DIRECTION ( 'NONE',  ( 0.000000000000000000, 1.000000000000000000, 0.000000000000000000 ) ) ;
#9119 = CARTESIAN_POINT ( 'NONE',  ( -25.55679448025485812, 2.417363203818269302, -207.9855790150824362 ) ) ;
#9120 = CC_DESIGN_SECURITY_CLASSIFICATION ( #11099, ( #11824 ) ) ;
#9121 = CARTESIAN_POINT ( 'NONE',  ( 8.935548306764875548, 10.16392762569079800, 2.855381327240379630 ) ) ;
#9122 = CARTESIAN_POINT ( 'NONE',  ( -0.06526978513835804407, 5.000000000000000888, -101.7940732946829598 ) ) ;
#9123 = CARTESIAN_POINT ( 'NONE',  ( 2.298097038856279362, 14.37500000000000000, -1.201902961143720860 ) ) ;
#9124 = AXIS2_PLACEMENT_3D ( 'NONE', #1758, #11182, #4542 ) ;
#9125 = EDGE_CURVE ( 'NONE', #2807, #2289, #12919, .T. ) ;
#9126 = DIRECTION ( 'NONE',  ( 0.000000000000000000, 0.000000000000000000, 1.000000000000000000 ) ) ;
#9127 = CARTESIAN_POINT ( 'NONE',  ( -2.651650429449552870, 0.6250000000000002220, -0.8483495705504463524 ) ) ;
#9128 =( BOUNDED_CURVE ( )  B_SPLINE_CURVE ( 3, ( #1398, #7417, #2796, #4872 ),
 .UNSPECIFIED., .F., .F. ) 
 B_SPLINE_CURVE_WITH_KNOTS ( ( 4, 4 ),
 ( 3.902948386497334887, 5.926982624441428094 ),
 .UNSPECIFIED. ) 
 CURVE ( )  GEOMETRIC_REPRESENTATION_ITEM ( )  RATIONAL_B_SPLINE_CURVE ( ( 1.000000000000000000, 0.6867676532959785529, 0.6867676532959785529, 1.000000000000000000 ) ) 
 REPRESENTATION_ITEM ( '' )  );
#9129 = DIRECTION ( 'NONE',  ( 0.000000000000000000, 0.000000000000000000, -1.000000000000000000 ) ) ;
#9130 = EDGE_CURVE ( 'NONE', #9880, #11483, #8976, .T. ) ;
#9131 = CARTESIAN_POINT ( 'NONE',  ( -6.269035454201815405, 12.12141402271314305, -125.0025068202018019 ) ) ;
#9132 = CARTESIAN_POINT ( 'NONE',  ( -1.346194077712559389, 14.43750000000000000, -6.749999999999999112 ) ) ;
#9133 = CARTESIAN_POINT ( 'NONE',  ( -5.142992306533066937, 10.00000000000000178, -113.9900399291647659 ) ) ;
#9134 = SECURITY_CLASSIFICATION ( '', '', #10539 ) ;
#9135 = CARTESIAN_POINT ( 'NONE',  ( 8.990525241558630754, 12.49999999999999822, 0.3362996048474836686 ) ) ;
#9136 = CARTESIAN_POINT ( 'NONE',  ( -3.249999999999999556, 9.187500000000000000, -2.153805922287440833 ) ) ;
#9137 = CIRCLE ( 'NONE', #13358, 3.500000000000000000 ) ;
#9138 = FACE_OUTER_BOUND ( 'NONE', #11548, .T. ) ;
#9139 = PLANE ( 'NONE',  #1724 ) ;
#9140 = VERTEX_POINT ( 'NONE', #9618 ) ;
#9141 = EDGE_LOOP ( 'NONE', ( #949, #8139, #6199, #6543 ) ) ;
#9142 = CARTESIAN_POINT ( 'NONE',  ( 30.32986759126112730, 0.7500000000000000000, 43.04214087805580391 ) ) ;
#9143 = CARTESIAN_POINT ( 'NONE',  ( -1.553300858899106629, 2.062500000000000000, 0.2500000000000002220 ) ) ;
#9144 = CARTESIAN_POINT ( 'NONE',  ( -3.249999999999999112, 14.68750000000000178, -2.153805922287440833 ) ) ;
#9145 = DIRECTION ( 'NONE',  ( 0.000000000000000000, -1.000000000000000000, 0.000000000000000000 ) ) ;
#9146 = ORIENTED_EDGE ( 'NONE', *, *, #3152, .T. ) ;
#9147 = CARTESIAN_POINT ( 'NONE',  ( 0.000000000000000000, 15.00000000000000000, -0.2500000000000002220 ) ) ;
#9148 = AXIS2_PLACEMENT_3D ( 'NONE', #11078, #2823, #8525 ) ;
#9149 = CARTESIAN_POINT ( 'NONE',  ( 9.948146083160592568, 11.56847231179307300, -43.54255919497041560 ) ) ;
#9150 = VECTOR ( 'NONE', #13796, 1000.000000000000114 ) ;
#9151 = EDGE_CURVE ( 'NONE', #3245, #9933, #4955, .T. ) ;
#9152 = AXIS2_PLACEMENT_3D ( 'NONE', #8716, #13452, #5245 ) ;
#9153 = CARTESIAN_POINT ( 'NONE',  ( -65.53364736412719083, 10.00000000000000000, -203.4171941195418754 ) ) ;
#9154 = CARTESIAN_POINT ( 'NONE',  ( -4.873637833193480873, 15.00000000000000000, -117.2491930705805885 ) ) ;
#9155 = CONTEXT_DEPENDENT_SHAPE_REPRESENTATION ( #10841, #2142 ) ;
#9156 = CARTESIAN_POINT ( 'NONE',  ( 10.12352296778766814, 15.00000000000000000, -125.3801087895597135 ) ) ;
#9157 = CARTESIAN_POINT ( 'NONE',  ( -7.472766077161554499, 14.05285657010038847, -116.8715385114339824 ) ) ;
#9158 = VERTEX_POINT ( 'NONE', #5761 ) ;
#9159 = CARTESIAN_POINT ( 'NONE',  ( 25.18430511132843108, 1.421781986552433485, -138.4549000095262272 ) ) ;
#9160 = CARTESIAN_POINT ( 'NONE',  ( -2.298097038856278918, 11.37500000000000000, -5.798097038856277585 ) ) ;
#9161 = AXIS2_PLACEMENT_3D ( 'NONE', #11024, #512, #3839 ) ;
#9162 = ORIENTED_EDGE ( 'NONE', *, *, #4578, .T. ) ;
#9163 = ORIENTED_EDGE ( 'NONE', *, *, #14614, .T. ) ;
#9164 = CARTESIAN_POINT ( 'NONE',  ( 0.000000000000000000, 5.000000000000000000, -0.2500000000000002220 ) ) ;
#9165 = CARTESIAN_POINT ( 'NONE',  ( 8.861879677533035959, 12.49999999999999822, -108.3481013197220619 ) ) ;
#9166 = CARTESIAN_POINT ( 'NONE',  ( 3.750000000000000000, 0.3125000000000002220, -1.946699141100892705 ) ) ;
#9167 = CARTESIAN_POINT ( 'NONE',  ( -1.346194077712558945, 6.562500000000000888, -0.2500000000000002220 ) ) ;
#9168 = VERTEX_POINT ( 'NONE', #10779 ) ;
#9169 = DIRECTION ( 'NONE',  ( 0.000000000000000000, 0.000000000000000000, -1.000000000000000000 ) ) ;
#9170 = DIRECTION ( 'NONE',  ( 0.000000000000000000, 0.000000000000000000, 1.000000000000000000 ) ) ;
#9171 = CARTESIAN_POINT ( 'NONE',  ( -1.553300858899106629, 6.062500000000000000, 0.2500000000000002220 ) ) ;
#9172 = AXIS2_PLACEMENT_3D ( 'NONE', #9475, #15223, #12654 ) ;
#9173 = CARTESIAN_POINT ( 'NONE',  ( -24.79172285805294251, 2.627299923518312763, -208.0710315741841043 ) ) ;
#9174 = DIRECTION ( 'NONE',  ( 0.000000000000000000, -1.000000000000000000, 0.000000000000000000 ) ) ;
#9175 = APPROVAL_ROLE ( '' ) ;
#9176 = CARTESIAN_POINT ( 'NONE',  ( 8.305394803915289614, 5.000000000000000888, -114.0089953534778004 ) ) ;
#9177 = ORIENTED_EDGE ( 'NONE', *, *, #7217, .F. ) ;
#9178 = CARTESIAN_POINT ( 'NONE',  ( -3.249999999999999112, 5.812500000000000888, -4.846194077712558723 ) ) ;
#9179 = AXIS2_PLACEMENT_3D ( 'NONE', #6207, #10922, #5054 ) ;
#9180 = PLANE ( 'NONE',  #4525 ) ;
#9181 = CARTESIAN_POINT ( 'NONE',  ( 3.749999999999999112, 11.31250000000000355, -1.946699141100893149 ) ) ;
#9182 = CARTESIAN_POINT ( 'NONE',  ( 0.000000000000000000, 14.00000000000000000, 0.2500000000000002220 ) ) ;
#9183 = CARTESIAN_POINT ( 'NONE',  ( 1.052436484934206939, 2.075239479414269894, -1.000000000000028644 ) ) ;
#9184 = CARTESIAN_POINT ( 'NONE',  ( -2.263856268268321870, 0.5959694101612306172, -137.7878962296450140 ) ) ;
#9185 = CARTESIAN_POINT ( 'NONE',  ( -3.750000000000000000, 12.81250000000000178, -5.053300858899105741 ) ) ;
#9186 = CARTESIAN_POINT ( 'NONE',  ( -3.435988495369542761, 4.336808689942017736E-16, -118.2234283277027487 ) ) ;
#9187 = SECURITY_CLASSIFICATION ( '', '', #11336 ) ;
#9188 = CARTESIAN_POINT ( 'NONE',  ( 9.958563954548985464, 4.811570552143352941, -44.18269933957010664 ) ) ;
#9189 = ORIENTED_EDGE ( 'NONE', *, *, #13876, .F. ) ;
#9190 = CARTESIAN_POINT ( 'NONE',  ( -27.59894172905100973, 3.999999999999963585, -206.0619156399042993 ) ) ;
#9191 = CARTESIAN_POINT ( 'NONE',  ( -3.249999999999999556, 0.3125000000000000555, -4.846194077712557835 ) ) ;
#9192 = ADVANCED_FACE ( 'NONE', ( #3367 ), #11297, .T. ) ;
#9193 = CIRCLE ( 'NONE', #9972, 2.326940983401415419 ) ;
#9194 = CARTESIAN_POINT ( 'NONE',  ( -56.64898049675471015, 9.999999999999998224, -176.0284089207397358 ) ) ;
#9195 = EDGE_CURVE ( 'NONE', #4732, #273, #8611, .T. ) ;
#9196 = CARTESIAN_POINT ( 'NONE',  ( 0.000000000000000000, 2.500000000000000000, -0.2500000000000002220 ) ) ;
#9197 = ORIENTED_EDGE ( 'NONE', *, *, #8680, .F. ) ;
#9198 = CARTESIAN_POINT ( 'NONE',  ( 1.756204145889998625, -2.540697700116526736, -1.000000000000007772 ) ) ;
#9199 = DIRECTION ( 'NONE',  ( 0.02181900108494737658, 0.000000000000000000, -0.9997619372588931741 ) ) ;
#9200 = CARTESIAN_POINT ( 'NONE',  ( 6.130230623468325035, 11.30611287585377589, 5.118568765223321826 ) ) ;
#9201 = CARTESIAN_POINT ( 'NONE',  ( -8.199037228203923888, -3.875321772615099985E-11, -114.3845095685870490 ) ) ;
#9202 = CARTESIAN_POINT ( 'NONE',  ( -3.980102097228897738E-16, 13.00000000000000000, -6.749999999999999112 ) ) ;
#9203 = FACE_OUTER_BOUND ( 'NONE', #8969, .T. ) ;
#9204 = CARTESIAN_POINT ( 'NONE',  ( -1.553300858899106629, 2.562500000000000444, 0.2500000000000002220 ) ) ;
#9205 = VECTOR ( 'NONE', #9870, 1000.000000000000000 ) ;
#9206 = DIRECTION ( 'NONE',  ( -0.9961255586397050887, 0.000000000000000000, 0.08794243244723005948 ) ) ;
#9207 = CARTESIAN_POINT ( 'NONE',  ( -6.435381799839732686, 15.00000000000000000, -129.7490639376177626 ) ) ;
#9208 = CARTESIAN_POINT ( 'NONE',  ( 21.22030245073296228, 8.195043764685355780E-16, -138.8546042205708773 ) ) ;
#9209 = CARTESIAN_POINT ( 'NONE',  ( 3.263686447136663116, 10.81848946384218912, 5.150370076467488012 ) ) ;
#9210 = CARTESIAN_POINT ( 'NONE',  ( 1.346194077712560944, 8.937500000000001776, -0.2500000000000010547 ) ) ;
#9211 = CARTESIAN_POINT ( 'NONE',  ( -8.959045066952105785, 11.66127071243621316, -104.5743688023792828 ) ) ;
#9212 = CARTESIAN_POINT ( 'NONE',  ( -3.955596480971199203, 9.999999999999998224, -118.5438621456188173 ) ) ;
#9213 = ORIENTED_EDGE ( 'NONE', *, *, #2154, .F. ) ;
#9214 = ORIENTED_EDGE ( 'NONE', *, *, #2692, .T. ) ;
#9215 = CARTESIAN_POINT ( 'NONE',  ( -13.51590403952440234, 1.734723475976807094E-15, -183.0154514670591936 ) ) ;
#9216 = CARTESIAN_POINT ( 'NONE',  ( -4.592425496802573972E-16, 5.500000000000000000, -7.249999999999999112 ) ) ;
#9217 = CIRCLE ( 'NONE', #346, 2.326940983401415419 ) ;
#9218 = CARTESIAN_POINT ( 'NONE',  ( -3.980102097228897738E-16, 14.00000000000000000, -6.749999999999999112 ) ) ;
#9219 = EDGE_CURVE ( 'NONE', #881, #1120, #1876, .T. ) ;
#9220 = CARTESIAN_POINT ( 'NONE',  ( -65.53364736412719083, 10.00000000000000000, -203.4171941195418754 ) ) ;
#9221 = VERTEX_POINT ( 'NONE', #9704 ) ;
#9222 =( BOUNDED_SURFACE ( )  B_SPLINE_SURFACE ( 3, 2, ( 
 ( #13929, #15175, #10217 ),
 ( #9121, #3170, #10285 ),
 ( #11444, #3400, #867 ),
 ( #5570, #12607, #9200 ),
 ( #1087, #15097, #14951 ),
 ( #2172, #11521, #4491 ),
 ( #4346, #9277, #8109 ),
 ( #12913, #6876, #8037 ),
 ( #12836, #5718, #14074 ),
 ( #937, #2326, #7025 ),
 ( #10437, #6952, #4412 ),
 ( #13775, #11739, #4568 ),
 ( #11670, #2098, #7961 ),
 ( #10514, #5794, #6732 ),
 ( #15021, #3249, #15250 ),
 ( #6805, #10356, #9053 ),
 ( #4640, #9350, #7882 ),
 ( #2022, #2628, #3554 ) ),
 .UNSPECIFIED., .F., .F., .T. ) 
 B_SPLINE_SURFACE_WITH_KNOTS ( ( 4, 2, 2, 2, 2, 2, 2, 2, 4 ),
 ( 3, 3 ),
 ( 0.01045536940180365887, 0.01094738860842426123, 0.01143940781504486186, 0.01193142702166546248, 0.01242344622828606485, 0.01291546543490666547, 0.01340748464152726610, 0.01389950384814786846, 0.01439152305476846909 ),
 ( 0.000000000000000000, 1.000000000000000000 ),
 .UNSPECIFIED. ) 
 GEOMETRIC_REPRESENTATION_ITEM ( )  RATIONAL_B_SPLINE_SURFACE ( (
 ( 1.000000000000000000, 0.6694682279269850156, 1.000000000000000000),
 ( 1.000000000000000000, 0.6694691252012310301, 1.000000000000000000),
 ( 1.000000000000000000, 0.6695768079868921197, 1.000000000000000000),
 ( 1.000000000000000000, 0.6700344632551947788, 1.000000000000000000),
 ( 1.000000000000000000, 0.6703764894997463752, 1.000000000000000000),
 ( 1.000000000000000000, 0.6713200582808653838, 1.000000000000000000),
 ( 1.000000000000000000, 0.6719288413528142767, 1.000000000000000000),
 ( 1.000000000000000000, 0.6734679306280143551, 1.000000000000000000),
 ( 1.000000000000000000, 0.6743949249898886222, 1.000000000000000000),
 ( 1.000000000000000000, 0.6766890287557600914, 1.000000000000000000),
 ( 1.000000000000000000, 0.6780280999877503767, 1.000000000000000000),
 ( 1.000000000000000000, 0.6812929544910970581, 1.000000000000000000),
 ( 1.000000000000000000, 0.6832424793221053561, 1.000000000000000000),
 ( 1.000000000000000000, 0.6879706062521270260, 1.000000000000000000),
 ( 1.000000000000000000, 0.6907332617435087974, 1.000000000000000000),
 ( 1.000000000000000000, 0.6976599582870975924, 1.000000000000000000),
 ( 1.000000000000000000, 0.7018653012264122193, 1.000000000000000000),
 ( 1.000000000000000000, 0.7071067811865473507, 1.000000000000000000) ) ) 
 REPRESENTATION_ITEM ( '' )  SURFACE ( )  );
#9223 = CARTESIAN_POINT ( 'NONE',  ( -3.980102097228897738E-16, 1.000000000000000000, -6.749999999999999112 ) ) ;
#9224 = CARTESIAN_POINT ( 'NONE',  ( -56.93825309386823363, 9.999999999999998224, -152.5131710537346805 ) ) ;
#9225 = FACE_OUTER_BOUND ( 'NONE', #6218, .T. ) ;
#9226 = DIRECTION ( 'NONE',  ( 0.000000000000000000, 0.000000000000000000, 1.000000000000000000 ) ) ;
#9227 = CARTESIAN_POINT ( 'NONE',  ( 2.298097038856278473, 5.625000000000000000, -5.798097038856279362 ) ) ;
#9228 = PERSON_AND_ORGANIZATION_ROLE ( 'classification_officer' ) ;
#9229 = VECTOR ( 'NONE', #4140, 1000.000000000000000 ) ;
#9230 = CC_DESIGN_PERSON_AND_ORGANIZATION_ASSIGNMENT ( #9606, #108, ( #12585 ) ) ;
#9231 = B_SPLINE_CURVE_WITH_KNOTS ( 'NONE', 3,
 ( #4031, #6489, #5260, #6412, #8886, #12441 ),
 .UNSPECIFIED., .F., .F.,
 ( 4, 2, 4 ),
 ( 1.734723475976807094E-18, 0.006358156888686363438, 0.01271631377737272514 ),
 .UNSPECIFIED. ) ;
#9232 = FACE_BOUND ( 'NONE', #11478, .T. ) ;
#9233 = CARTESIAN_POINT ( 'NONE',  ( -4.924212822021372560, 14.97043413793575972, -117.3690025739556404 ) ) ;
#9234 = ORIENTED_EDGE ( 'NONE', *, *, #1189, .F. ) ;
#9235 = CARTESIAN_POINT ( 'NONE',  ( 25.92117664022351420, 2.488669359944063242, -137.1713175122655173 ) ) ;
#9236 = CARTESIAN_POINT ( 'NONE',  ( 0.000000000000000000, 12.00000000000000000, -0.2500000000000002220 ) ) ;
#9237 = ORIENTED_EDGE ( 'NONE', *, *, #13666, .F. ) ;
#9238 = ADVANCED_FACE ( 'NONE', ( #3104, #12088 ), #2673, .T. ) ;
#9239 = VERTEX_POINT ( 'NONE', #10855 ) ;
#9240 = CARTESIAN_POINT ( 'NONE',  ( -3.749999999999999556, 11.75000000000000178, -3.499999999999999112 ) ) ;
#9241 = DIRECTION ( 'NONE',  ( 0.000000000000000000, 0.000000000000000000, -1.000000000000000000 ) ) ;
#9242 = CARTESIAN_POINT ( 'NONE',  ( -3.750000000000000000, 2.812500000000000444, -5.053300858899105741 ) ) ;
#9243 = EDGE_CURVE ( 'NONE', #9630, #5655, #9783, .T. ) ;
#9244 = CARTESIAN_POINT ( 'NONE',  ( 3.249999999999998224, 7.312500000000001776, -2.153805922287439945 ) ) ;
#9246 = EDGE_CURVE ( 'NONE', #12872, #2589, #357, .T. ) ;
#9245 = EDGE_LOOP ( 'NONE', ( #2218, #4598, #7364 ) ) ;
#9247 = CARTESIAN_POINT ( 'NONE',  ( -6.442579204135082449, 14.53778547989058723, -116.6257450304697585 ) ) ;
#9248 = CIRCLE ( 'NONE', #6532, 2.500000000000000000 ) ;
#9249 = CARTESIAN_POINT ( 'NONE',  ( -3.980102097228897245E-16, 3.500000000000000000, -6.749999999999999112 ) ) ;
#9250 = CARTESIAN_POINT ( 'NONE',  ( 2.651650429449552870, 7.625000000000000000, -6.151650429449554203 ) ) ;
#9251 = CARTESIAN_POINT ( 'NONE',  ( -25.43638953643460354, 0.8166224425976650325, -205.4887980176190752 ) ) ;
#9252 = CYLINDRICAL_SURFACE ( 'NONE', #5475, 6.999999999999950262 ) ;
#9253 = DATE_TIME_ROLE ( 'classification_date' ) ;
#9254 = CARTESIAN_POINT ( 'NONE',  ( 10.77011162811585265, 5.000000000000002665, -107.4112503379939056 ) ) ;
#9255 = ORIENTED_EDGE ( 'NONE', *, *, #7302, .T. ) ;
#9256 = CARTESIAN_POINT ( 'NONE',  ( -1.346194077712559167, 5.937500000000000000, -6.749999999999999112 ) ) ;
#9257 = FACE_OUTER_BOUND ( 'NONE', #4262, .T. ) ;
#9258 = PRODUCT_DEFINITION ( 'UNKNOWN', '', #8939, #14716 ) ;
#9259 = CARTESIAN_POINT ( 'NONE',  ( 3.749999999999999112, 10.31250000000000000, -1.946699141100893149 ) ) ;
#9260 = CARTESIAN_POINT ( 'NONE',  ( -2.651650429449552870, 13.12500000000000000, -0.8483495705504462414 ) ) ;
#9261 = CARTESIAN_POINT ( 'NONE',  ( -63.60348060676461301, 15.00000000000000000, -180.2685449772604045 ) ) ;
#9262 = CARTESIAN_POINT ( 'NONE',  ( -0.1260096660175019090, -0.1954009359728117456, 0.1491815183709511716 ) ) ;
#9263 = CARTESIAN_POINT ( 'NONE',  ( -3.249999999999999556, 8.187500000000000000, -2.153805922287440833 ) ) ;
#9264 = CARTESIAN_POINT ( 'NONE',  ( -3.249999999999999112, -0.1874999999999998890, -4.846194077712558723 ) ) ;
#9265 = CARTESIAN_POINT ( 'NONE',  ( -2.783652268060036850, 4.336808689942017736E-16, -111.2342432958199367 ) ) ;
#9266 =( REPRESENTATION_RELATIONSHIP ('NONE','NONE', #11394, #9314 ) REPRESENTATION_RELATIONSHIP_WITH_TRANSFORMATION ( #1117 )SHAPE_REPRESENTATION_RELATIONSHIP( ) );
#9267 = PERSON_AND_ORGANIZATION_ROLE ( 'creator' ) ;
#9268 = CARTESIAN_POINT ( 'NONE',  ( -22.00712180358226533, 9.999999999999998224, -133.4290821151669206 ) ) ;
#9269 = EDGE_LOOP ( 'NONE', ( #8860, #5854, #579, #8583 ) ) ;
#9270 = CARTESIAN_POINT ( 'NONE',  ( 8.640721352953065093, 3.280814622354975452, 2.680269431086986121 ) ) ;
#9271 = CARTESIAN_POINT ( 'NONE',  ( 1.346194077712560944, 3.937500000000000000, -0.2500000000000011102 ) ) ;
#9272 = CARTESIAN_POINT ( 'NONE',  ( -65.95211062277772385, 15.00000000000000000, -188.5353794584724483 ) ) ;
#9273 = CARTESIAN_POINT ( 'NONE',  ( 3.249999999999999556, 2.249999999999999556, -3.500000000000000000 ) ) ;
#9274 = VERTEX_POINT ( 'NONE', #3991 ) ;
#9275 = FACE_OUTER_BOUND ( 'NONE', #5047, .T. ) ;
#9276 = FACE_OUTER_BOUND ( 'NONE', #13734, .T. ) ;
#9277 = CARTESIAN_POINT ( 'NONE',  ( 8.890868772111733875, 12.65371242469951341, 4.902628950838662014 ) ) ;
#9278 = CARTESIAN_POINT ( 'NONE',  ( -0.5126277339370232111, 5.000000000000000888, -103.6859198938564646 ) ) ;
#9279 = CARTESIAN_POINT ( 'NONE',  ( -3.249999999999999112, 11.68749999999999822, -2.153805922287440833 ) ) ;
#9281 = EDGE_CURVE ( 'NONE', #1413, #10593, #9723, .T. ) ;
#9280 = DIRECTION ( 'NONE',  ( 0.9997619372588932851, 0.000000000000000000, 0.02181900108494707127 ) ) ;
#9282 = CARTESIAN_POINT ( 'NONE',  ( 0.000000000000000000, 0.5000000000000001110, 0.2500000000000002220 ) ) ;
#9283 = FACE_OUTER_BOUND ( 'NONE', #11461, .T. ) ;
#9284 = CARTESIAN_POINT ( 'NONE',  ( -7.676911175420229050, 13.35713519559141638, -104.8728676159044966 ) ) ;
#9285 = CARTESIAN_POINT ( 'NONE',  ( -9.541039381253360929, 10.00000000000000355, -124.0820960698317066 ) ) ;
#9286 = CARTESIAN_POINT ( 'NONE',  ( -4.841311305102414586, 2.099999999999999645, 31.26088239576554173 ) ) ;
#9287 = CARTESIAN_POINT ( 'NONE',  ( -2.298097038856278473, 13.12500000000000000, -1.201902961143720416 ) ) ;
#9288 = CARTESIAN_POINT ( 'NONE',  ( -6.328185151855761248, 14.51326209089783248, -103.7941250579298895 ) ) ;
#9289 = DIRECTION ( 'NONE',  ( 0.000000000000000000, -1.000000000000000000, 0.000000000000000000 ) ) ;
#9290 = EDGE_LOOP ( 'NONE', ( #13699, #12224, #10595, #11536 ) ) ;
#9291 = ORIENTED_EDGE ( 'NONE', *, *, #14807, .T. ) ;
#9292 = CARTESIAN_POINT ( 'NONE',  ( -0.3766621274091715987, -0.2500000000000000000, -7.146945437571387671 ) ) ;
#9293 = CARTESIAN_POINT ( 'NONE',  ( 1.553300858899108849, 5.937500000000000000, 0.2499999999999993616 ) ) ;
#9294 = CARTESIAN_POINT ( 'NONE',  ( -1.553300858899106629, 5.562500000000000000, 0.2499999999999998335 ) ) ;
#9295 = CARTESIAN_POINT ( 'NONE',  ( -7.414180893040303921, 4.336808689942017736E-16, -103.4903665579796410 ) ) ;
#9296 = ORIENTED_EDGE ( 'NONE', *, *, #9989, .F. ) ;
#9297 = CARTESIAN_POINT ( 'NONE',  ( -2.298097038856279362, 1.874999999999999778, -5.798097038856278473 ) ) ;
#9298 = EDGE_CURVE ( 'NONE', #12551, #10617, #435, .T. ) ;
#9299 = CARTESIAN_POINT ( 'NONE',  ( -50.48705678711692002, 15.00000000000000000, -152.0942671431891142 ) ) ;
#9300 = VECTOR ( 'NONE', #3875, 1000.000000000000114 ) ;
#9301 = CARTESIAN_POINT ( 'NONE',  ( 5.475206276408092876, 0.000000000000000000, -34.56909192082981974 ) ) ;
#9302 = ADVANCED_FACE ( 'NONE', ( #5144 ), #10137, .T. ) ;
#9303 = CARTESIAN_POINT ( 'NONE',  ( -1.346194077712559389, 2.437500000000000444, -6.749999999999999112 ) ) ;
#9304 = SECURITY_CLASSIFICATION_LEVEL ( 'unclassified' ) ;
#9305 = DIRECTION ( 'NONE',  ( -0.000000000000000000, -1.000000000000000000, -0.000000000000000000 ) ) ;
#9306 = DIRECTION ( 'NONE',  ( 0.08794243244722413366, 0.000000000000000000, 0.9961255586397056438 ) ) ;
#9307 = EDGE_LOOP ( 'NONE', ( #3287, #8610, #2190, #264 ) ) ;
#9308 = CARTESIAN_POINT ( 'NONE',  ( -7.768256104199515732, 15.00000000000000000, -129.7494471864078491 ) ) ;
#9309 = CARTESIAN_POINT ( 'NONE',  ( 2.298097038856278473, 10.62500000000000000, -5.798097038856279362 ) ) ;
#9310 = ORIENTED_EDGE ( 'NONE', *, *, #14699, .T. ) ;
#9311 = VERTEX_POINT ( 'NONE', #7535 ) ;
#9312 = CARTESIAN_POINT ( 'NONE',  ( 1.553300858899109516, 9.437500000000000000, 0.2499999999999993616 ) ) ;
#9313 = CARTESIAN_POINT ( 'NONE',  ( -27.47952516445719695, 4.000000000000000888, -206.2928504520293131 ) ) ;
#9314 = SHAPE_REPRESENTATION ( 'SmallSpring', ( #9419 ), #6710 ) ;
#9315 = CARTESIAN_POINT ( 'NONE',  ( 0.000000000000000000, 7.500000000000000888, 0.2500000000000002220 ) ) ;
#9316 = AXIS2_PLACEMENT_3D ( 'NONE', #4820, #10767, #14335 ) ;
#9317 = CARTESIAN_POINT ( 'NONE',  ( 3.249999999999999556, 8.250000000000000000, -3.500000000000000000 ) ) ;
#9318 = ORIENTED_EDGE ( 'NONE', *, *, #10561, .T. ) ;
#9319 = CARTESIAN_POINT ( 'NONE',  ( -0.8896971555397489295, 9.999999999999998224, -104.6801027822219936 ) ) ;
#9320 = CARTESIAN_POINT ( 'NONE',  ( -3.249999999999999556, 3.312500000000000000, -4.846194077712557835 ) ) ;
#9321 = CARTESIAN_POINT ( 'NONE',  ( -3.749999999999999556, 4.312500000000000888, -5.053300858899104853 ) ) ;
#9322 = CARTESIAN_POINT ( 'NONE',  ( -25.12160904166909958, 2.323552219295974108, -208.4222310589716471 ) ) ;
#9323 = EDGE_CURVE ( 'NONE', #2594, #7276, #3295, .T. ) ;
#9324 = CARTESIAN_POINT ( 'NONE',  ( 1.818748563159308773, 10.00000000000000178, -137.3269871014800003 ) ) ;
#9325 = EDGE_CURVE ( 'NONE', #11802, #8895, #85, .T. ) ;
#9326 = FACE_OUTER_BOUND ( 'NONE', #13694, .T. ) ;
#9327 = PERSON_AND_ORGANIZATION ( #3176, #3020 ) ;
#9328 = EDGE_CURVE ( 'NONE', #3650, #814, #12763, .T. ) ;
#9329 = FACE_OUTER_BOUND ( 'NONE', #11256, .T. ) ;
#9330 = DIRECTION ( 'NONE',  ( 0.000000000000000000, 0.000000000000000000, 1.000000000000000000 ) ) ;
#9331 = ORIENTED_EDGE ( 'NONE', *, *, #4783, .F. ) ;
#9332 = CARTESIAN_POINT ( 'NONE',  ( -3.980102097228897738E-16, 8.000000000000000000, -6.749999999999999112 ) ) ;
#9333 = DIRECTION ( 'NONE',  ( 0.08794243244722427244, 0.000000000000000000, 0.9961255586397056438 ) ) ;
#9334 = CARTESIAN_POINT ( 'NONE',  ( -2.651650429449552870, 8.625000000000000000, -0.8483495705504467965 ) ) ;
#9335 = CARTESIAN_POINT ( 'NONE',  ( -3.750000000000000000, 12.31250000000000000, -5.053300858899105741 ) ) ;
#9336 = CARTESIAN_POINT ( 'NONE',  ( -66.92994642267662186, 14.64660082127883811, -194.1686397956628127 ) ) ;
#9337 = CARTESIAN_POINT ( 'NONE',  ( -0.2256904824989624803, 2.216033281584864678, -138.2198612530219179 ) ) ;
#9338 = CARTESIAN_POINT ( 'NONE',  ( -1.346194077712559167, -0.06249999999999988898, -6.749999999999999112 ) ) ;
#9339 = DIRECTION ( 'NONE',  ( -0.000000000000000000, -1.000000000000000000, -0.000000000000000000 ) ) ;
#9340 = ADVANCED_FACE ( 'NONE', ( #14002 ), #9222, .T. ) ;
#9341 = SHAPE_DEFINITION_REPRESENTATION ( #3753, #11394 ) ;
#9342 = CARTESIAN_POINT ( 'NONE',  ( 9.943023108890811201, 5.000000000000000888, -43.30782091980646697 ) ) ;
#9343 = ORIENTED_EDGE ( 'NONE', *, *, #11314, .T. ) ;
#9344 = CARTESIAN_POINT ( 'NONE',  ( 0.3766621274091715987, -0.2500000000000000000, -6.863050255469941519 ) ) ;
#9345 = CARTESIAN_POINT ( 'NONE',  ( -1.346194077712558945, 2.062500000000000000, -0.2500000000000002220 ) ) ;
#9346 = CARTESIAN_POINT ( 'NONE',  ( 3.249999999999998224, 7.187500000000000888, -4.846194077712561388 ) ) ;
#9347 = ORIENTED_EDGE ( 'NONE', *, *, #3758, .F. ) ;
#9348 = CARTESIAN_POINT ( 'NONE',  ( 1.052436484934852201, -2.165641995260652486, -1.000000000000001110 ) ) ;
#9349 = FACE_OUTER_BOUND ( 'NONE', #1475, .T. ) ;
#9350 = CARTESIAN_POINT ( 'NONE',  ( 8.983776437537306592, 15.03735113318141714, 0.6455345399050246291 ) ) ;
#9351 = CARTESIAN_POINT ( 'NONE',  ( -3.249999999999999112, 10.81250000000000000, -4.846194077712558723 ) ) ;
#9352 = CARTESIAN_POINT ( 'NONE',  ( 8.536856906383286869, 0.000000000000000000, -164.4613227688425354 ) ) ;
#9353 = CARTESIAN_POINT ( 'NONE',  ( -1.553300858899107073, 2.937500000000000444, -7.249999999999999112 ) ) ;
#9354 = CARTESIAN_POINT ( 'NONE',  ( -8.205916711996726676, 7.499999999999991118, -92.94857034792688921 ) ) ;
#9355 = DIRECTION ( 'NONE',  ( 1.000000000000000000, 0.000000000000000000, 0.000000000000000000 ) ) ;
#9356 = CARTESIAN_POINT ( 'NONE',  ( 25.98238260393377175, 2.581044006060433382, -137.1487496856579753 ) ) ;
#9357 = CARTESIAN_POINT ( 'NONE',  ( -5.599503270685788792, 0.000000000000000000, 20.51657426689472885 ) ) ;
#9358 = CARTESIAN_POINT ( 'NONE',  ( -2.298097038856278918, 11.37500000000000000, -5.798097038856277585 ) ) ;
#9359 = CARTESIAN_POINT ( 'NONE',  ( 30.32986759126112730, 0.000000000000000000, 41.04214087805579680 ) ) ;
#9360 = CARTESIAN_POINT ( 'NONE',  ( -63.68025975125228655, 12.30547768668273001, -202.4996554109041540 ) ) ;
#9361 = EDGE_LOOP ( 'NONE', ( #11754, #6148, #11823 ) ) ;
#9362 = ORIENTED_EDGE ( 'NONE', *, *, #2194, .F. ) ;
#9363 = CARTESIAN_POINT ( 'NONE',  ( 9.653464198873995983, 12.50000000000000000, -108.9308074128229862 ) ) ;
#9364 = CARTESIAN_POINT ( 'NONE',  ( -2.651650429449552870, 5.125000000000000000, -0.8483495705504462414 ) ) ;
#9365 = CARTESIAN_POINT ( 'NONE',  ( -2.651650429449552870, 5.875000000000000888, -6.151650429449552426 ) ) ;
#9366 = DIRECTION ( 'NONE',  ( 0.000000000000000000, 1.000000000000000000, 0.000000000000000000 ) ) ;
#9367 = ORIENTED_EDGE ( 'NONE', *, *, #2974, .F. ) ;
#9368 = CARTESIAN_POINT ( 'NONE',  ( 3.249999999999999556, 1.249999999999999778, -3.500000000000000000 ) ) ;
#9369 = CARTESIAN_POINT ( 'NONE',  ( -55.30796743870962473, 9.999999999999998224, -150.1894123919774700 ) ) ;
#9370 = SECURITY_CLASSIFICATION ( '', '', #7540 ) ;
#9371 = CARTESIAN_POINT ( 'NONE',  ( 1.500000000000000000, 4.500000000000000888, 0.2500000000000002220 ) ) ;
#9372 =( NAMED_UNIT ( * ) PLANE_ANGLE_UNIT ( ) SI_UNIT ( $, .RADIAN. ) );
#9373 = CARTESIAN_POINT ( 'NONE',  ( 2.298097038856279362, 2.875000000000000000, -1.201902961143720860 ) ) ;
#9374 = AXIS2_PLACEMENT_3D ( 'NONE', #2051, #9006, #10246 ) ;
#9375 = DATE_AND_TIME ( #14027, #6171 ) ;
#9376 = DIRECTION ( 'NONE',  ( 0.000000000000000000, -1.000000000000000000, 0.000000000000000000 ) ) ;
#9377 = CARTESIAN_POINT ( 'NONE',  ( 13.35507181691441225, 0.000000000000000000, -132.8670847673578805 ) ) ;
#9378 = ORIENTED_EDGE ( 'NONE', *, *, #14507, .F. ) ;
#9379 = CARTESIAN_POINT ( 'NONE',  ( 11.32016196459912649, 15.00000000000000000, -106.4092894470390291 ) ) ;
#9380 = DIRECTION ( 'NONE',  ( 0.000000000000000000, 0.000000000000000000, -1.000000000000000000 ) ) ;
#9381 = ORIENTED_EDGE ( 'NONE', *, *, #10609, .T. ) ;
#9382 = EDGE_CURVE ( 'NONE', #9763, #13945, #832, .T. ) ;
#9383 = ADVANCED_FACE ( 'NONE', ( #3629 ), #3909, .T. ) ;
#9384 = ORIENTED_EDGE ( 'NONE', *, *, #14442, .F. ) ;
#9385 = CARTESIAN_POINT ( 'NONE',  ( -28.63722085524334204, 3.999999999999999112, -204.0000079243689868 ) ) ;
#9386 = CARTESIAN_POINT ( 'NONE',  ( -2.651650429449552870, 4.625000000000000888, -0.8483495705504463524 ) ) ;
#9387 = CARTESIAN_POINT ( 'NONE',  ( 3.249999999999998224, 5.312500000000000000, -2.153805922287439945 ) ) ;
#9388 = ORIENTED_EDGE ( 'NONE', *, *, #1558, .T. ) ;
#9389 = LOCAL_TIME ( 12, 28, 20.00000000000000000, #5594 ) ;
#9390 = ADVANCED_FACE ( 'NONE', ( #13300 ), #6016, .F. ) ;
#9391 = CARTESIAN_POINT ( 'NONE',  ( -3.899357168004182002E-10, 15.00000000000247624, -101.1952717268974311 ) ) ;
#9392 = TOROIDAL_SURFACE ( 'NONE', #3475, 11.99999999999994138, 5.000000000000000000 ) ;
#9393 = CARTESIAN_POINT ( 'NONE',  ( -3.980102097228897245E-16, 4.500000000000000888, -6.749999999999999112 ) ) ;
#9394 = AXIS2_PLACEMENT_3D ( 'NONE', #4725, #6100, #8193 ) ;
#9395 = VECTOR ( 'NONE', #5013, 1000.000000000000000 ) ;
#9396 = CARTESIAN_POINT ( 'NONE',  ( 3.749999999999999112, 8.812500000000000000, -1.946699141100892039 ) ) ;
#9397 = CARTESIAN_POINT ( 'NONE',  ( -25.33200545782566238, 0.2453806451254461896, -202.6873302614697252 ) ) ;
#9398 = CARTESIAN_POINT ( 'NONE',  ( 4.950900406836922230, 0.000000000000000000, -134.4284351762048573 ) ) ;
#9399 = CARTESIAN_POINT ( 'NONE',  ( -0.6421131273608509105, -2.743867526398025447, -43.87268297926051730 ) ) ;
#9400 = PERSON_AND_ORGANIZATION ( #3176, #3020 ) ;
#9401 = CIRCLE ( 'NONE', #7416, 2.000000000000001776 ) ;
#9402 = CARTESIAN_POINT ( 'NONE',  ( -0.01496453197141594735, 0.000000000000000000, -5.196130874293185542 ) ) ;
#9403 = CIRCLE ( 'NONE', #4715, 4.999999999999998224 ) ;
#9404 =( BOUNDED_SURFACE ( )  B_SPLINE_SURFACE ( 3, 1, ( 
 ( #9839, #9920 ),
 ( #8758, #649 ),
 ( #10069, #1717 ),
 ( #13329, #14804 ) ),
 .UNSPECIFIED., .F., .F., .F. ) 
 B_SPLINE_SURFACE_WITH_KNOTS ( ( 4, 4 ),
 ( 2, 2 ),
 ( 0.000000000000000000, 1.000000000000000000 ),
 ( 0.000000000000000000, 1.000000000000000000 ),
 .UNSPECIFIED. ) 
 GEOMETRIC_REPRESENTATION_ITEM ( )  RATIONAL_B_SPLINE_SURFACE ( (
 ( 1.000000000000000000, 1.000000000000000000),
 ( 0.9216682375510409919, 0.9216682375510409919),
 ( 0.9216682375510409919, 0.9216682375510409919),
 ( 1.000000000000000000, 1.000000000000000000) ) ) 
 REPRESENTATION_ITEM ( '' )  SURFACE ( )  );
#9405 = ORIENTED_EDGE ( 'NONE', *, *, #3387, .T. ) ;
#9406 = CARTESIAN_POINT ( 'NONE',  ( 3.249999999999998224, 7.312500000000000000, -2.153805922287439945 ) ) ;
#9407 = ADVANCED_FACE ( 'NONE', ( #3785 ), #8725, .T. ) ;
#9408 = CARTESIAN_POINT ( 'NONE',  ( 4.716951098700676859, 2.490287375297125294, -44.10818225254241298 ) ) ;
#9409 = CARTESIAN_POINT ( 'NONE',  ( -3.750000000000000000, 11.68749999999999822, -1.946699141100893149 ) ) ;
#9410 = CARTESIAN_POINT ( 'NONE',  ( -5.794432043291358525, 6.000000000000000000, -125.0404107129116085 ) ) ;
#9411 = CARTESIAN_POINT ( 'NONE',  ( 1.453757729950659217, 2.743867526398027223, -1.000000000000029088 ) ) ;
#9412 = CARTESIAN_POINT ( 'NONE',  ( 6.869258321017759350, -2.075239479414269894, -34.56909192082981974 ) ) ;
#9413 = CARTESIAN_POINT ( 'NONE',  ( -1.553300858899107073, 12.93750000000000178, -7.249999999999999112 ) ) ;
#9414 = DIRECTION ( 'NONE',  ( 0.9989498407774362043, 0.000000000000000000, 0.04581719776170026237 ) ) ;
#9415 = COORDINATED_UNIVERSAL_TIME_OFFSET ( 0, 0, .AHEAD. ) ;
#9416 = PRODUCT_DEFINITION_SHAPE ( 'NONE', 'NONE',  #15324 ) ;
#9417 = CARTESIAN_POINT ( 'NONE',  ( 3.249999999999999112, 14.81250000000000000, -2.153805922287439945 ) ) ;
#9418 = CARTESIAN_POINT ( 'NONE',  ( 0.000000000000000000, 0.000000000000000000, -6.000000000000002665 ) ) ;
#9419 = AXIS2_PLACEMENT_3D ( 'NONE', #15272, #9226, #12943 ) ;
#9420 = ORIENTED_EDGE ( 'NONE', *, *, #6390, .F. ) ;
#9421 = CARTESIAN_POINT ( 'NONE',  ( 8.875022499991118252, 5.000000000000000888, 5.628716256677545715 ) ) ;
#9422 = CARTESIAN_POINT ( 'NONE',  ( -2.298097038856278918, 1.375000000000000000, -5.798097038856277585 ) ) ;
#9423 = CARTESIAN_POINT ( 'NONE',  ( -7.004554049466862331, -1.494908006873514903E-15, -104.1936728214014636 ) ) ;
#9424 = CARTESIAN_POINT ( 'NONE',  ( -1.346194077712558945, 5.562500000000001776, -0.2500000000000002220 ) ) ;
#9425 = ORIENTED_EDGE ( 'NONE', *, *, #4053, .F. ) ;
#9426 = CARTESIAN_POINT ( 'NONE',  ( -5.997216956328301762, 9.999999999999998224, -109.1002327433092915 ) ) ;
#9427 = EDGE_CURVE ( 'NONE', #2695, #1413, #8952, .T. ) ;
#9428 = CARTESIAN_POINT ( 'NONE',  ( 0.4539486869273933189, 11.45452110608535179, 2.843399008810883366 ) ) ;
#9429 = CARTESIAN_POINT ( 'NONE',  ( 9.891575892914513446, 14.76107634086678644, -106.0971120608575120 ) ) ;
#9430 = CARTESIAN_POINT ( 'NONE',  ( 3.249999999999999112, 1.812500000000000222, -2.153805922287439945 ) ) ;
#9431 = CARTESIAN_POINT ( 'NONE',  ( 2.298097038856279362, 12.37500000000000178, -1.201902961143720860 ) ) ;
#9432 = CC_DESIGN_SECURITY_CLASSIFICATION ( #10180, ( #8939 ) ) ;
#9433 = CARTESIAN_POINT ( 'NONE',  ( 13.15367060044211556, 0.000000000000000000, -166.3809663071982641 ) ) ;
#9434 = CARTESIAN_POINT ( 'NONE',  ( -1.553300858899106629, 3.562500000000000888, 0.2500000000000002220 ) ) ;
#9435 = DIRECTION ( 'NONE',  ( -0.000000000000000000, -1.000000000000000000, -0.000000000000000000 ) ) ;
#9436 = CARTESIAN_POINT ( 'NONE',  ( -2.524281728693007043, 7.379999999999995453, -45.64919840677852392 ) ) ;
#9437 = DIRECTION ( 'NONE',  ( -0.000000000000000000, 1.000000000000000000, -0.000000000000000000 ) ) ;
#9438 = CARTESIAN_POINT ( 'NONE',  ( -25.68053481550299111, -5.000000000000000888, -142.4798935003980773 ) ) ;
#9439 = CARTESIAN_POINT ( 'NONE',  ( 2.298097038856278473, 11.62500000000000000, -5.798097038856279362 ) ) ;
#9440 = CARTESIAN_POINT ( 'NONE',  ( 52.73038795364751508, 1.750000000000000000, 69.25342193720584305 ) ) ;
#9441 = CARTESIAN_POINT ( 'NONE',  ( -64.64338443439244486, 14.97268095330599458, -185.5119884393937184 ) ) ;
#9442 = ORIENTED_EDGE ( 'NONE', *, *, #13475, .F. ) ;
#9443 = EDGE_LOOP ( 'NONE', ( #499, #9008 ) ) ;
#9444 = CARTESIAN_POINT ( 'NONE',  ( -4.724265062691370254, 4.336808689942017736E-16, -106.3929389433132400 ) ) ;
#9445 = CARTESIAN_POINT ( 'NONE',  ( -0.3766621274091715987, 0.5000000000000000000, -0.1347136637304948981 ) ) ;
#9446 = CARTESIAN_POINT ( 'NONE',  ( 3.749999999999999112, 4.812500000000000888, -1.946699141100892039 ) ) ;
#9447 = CARTESIAN_POINT ( 'NONE',  ( 3.749999999999999112, 5.312500000000000000, -1.946699141100893149 ) ) ;
#9448 = DIRECTION ( 'NONE',  ( 0.000000000000000000, 0.000000000000000000, 1.000000000000000000 ) ) ;
#9449 = ORIENTED_EDGE ( 'NONE', *, *, #4389, .F. ) ;
#9450 = CARTESIAN_POINT ( 'NONE',  ( -7.490165920340420946, 1.096071398114234263, -116.1895725676946682 ) ) ;
#9451 = ADVANCED_BREP_SHAPE_REPRESENTATION ( '', ( #2140, #9419 ), #3238 ) ;
#9452 = VECTOR ( 'NONE', #2530, 1000.000000000000000 ) ;
#9453 = CARTESIAN_POINT ( 'NONE',  ( -1.346194077712559389, 13.43749999999999822, -6.749999999999999112 ) ) ;
#9454 = CYLINDRICAL_SURFACE ( 'NONE', #3716, 1.000000000000000888 ) ;
#9455 = DIRECTION ( 'NONE',  ( 0.000000000000000000, 0.000000000000000000, 1.000000000000000000 ) ) ;
#9456 = CARTESIAN_POINT ( 'NONE',  ( -9.044950117654430244, -11.21819190899177343, 2.974682809436260289 ) ) ;
#9457 = CARTESIAN_POINT ( 'NONE',  ( -2.298097038856278473, 4.125000000000000000, -1.201902961143720416 ) ) ;
#9458 = DATE_AND_TIME ( #4743, #15076 ) ;
#9459 = CARTESIAN_POINT ( 'NONE',  ( 10.02128254425321607, 15.00000000000000000, -108.3753986617072371 ) ) ;
#9460 = CARTESIAN_POINT ( 'NONE',  ( 5.853739503561296686, 8.673617379884035472E-16, -123.2563334432540785 ) ) ;
#9461 = ORIENTED_EDGE ( 'NONE', *, *, #7320, .T. ) ;
#9462 = AXIS2_PLACEMENT_3D ( 'NONE', #12682, #1010, #3328 ) ;
#9463 = CARTESIAN_POINT ( 'NONE',  ( 2.219068112418553174, -2.193945312325717101, -1.000000000000001110 ) ) ;
#9464 = DIRECTION ( 'NONE',  ( 0.000000000000000000, -1.000000000000000000, 0.000000000000000000 ) ) ;
#9465 = ORIENTED_EDGE ( 'NONE', *, *, #5175, .T. ) ;
#9466 = ORIENTED_EDGE ( 'NONE', *, *, #5550, .F. ) ;
#9467 = CARTESIAN_POINT ( 'NONE',  ( 7.347880794884122694E-16, 0.000000000000000000, 6.000000000000002665 ) ) ;
#9468 = CARTESIAN_POINT ( 'NONE',  ( -2.651650429449552870, 5.625000000000000888, -0.8483495705504463524 ) ) ;
#9469 = CARTESIAN_POINT ( 'NONE',  ( -2.298097038856279362, 5.875000000000001776, -5.798097038856278473 ) ) ;
#9470 = ORIENTED_EDGE ( 'NONE', *, *, #8183, .F. ) ;
#9471 = CARTESIAN_POINT ( 'NONE',  ( 4.892302586673455522, 15.00000000000000000, -102.5092683516998875 ) ) ;
#9472 = CARTESIAN_POINT ( 'NONE',  ( 1.346194077712560944, 1.937500000000000000, -0.2500000000000010547 ) ) ;
#9473 = VECTOR ( 'NONE', #12515, 1000.000000000000000 ) ;
#9474 = CARTESIAN_POINT ( 'NONE',  ( -7.262467309341673172, 2.500000000000000444, -120.6566834617809008 ) ) ;
#9475 = CARTESIAN_POINT ( 'NONE',  ( 29.21736815051484015, 8.773889247172311556, -44.21329492081407153 ) ) ;
#9476 = LINE ( 'NONE', #11860, #11619 ) ;
#9477 = PERSON_AND_ORGANIZATION_ROLE ( 'design_supplier' ) ;
#9478 = CARTESIAN_POINT ( 'NONE',  ( 1.893911505664648054, 5.000000000000000888, -1.663006917529762152 ) ) ;
#9479 = B_SPLINE_CURVE_WITH_KNOTS ( 'NONE', 3,
 ( #10903, #13472, #9901, #2875 ),
 .UNSPECIFIED., .F., .F.,
 ( 4, 4 ),
 ( 4.512482785797534139E-18, 0.0003024267748246941591 ),
 .UNSPECIFIED. ) ;
#9480 = VERTEX_POINT ( 'NONE', #6257 ) ;
#9481 = VECTOR ( 'NONE', #4133, 1000.000000000000000 ) ;
#9482 = CARTESIAN_POINT ( 'NONE',  ( -4.878690035801932723, 0.000000000000000000, -0.3860167444088152822 ) ) ;
#9483 = CARTESIAN_POINT ( 'NONE',  ( -2.651650429449552870, 11.87500000000000000, -6.151650429449552426 ) ) ;
#9484 = CARTESIAN_POINT ( 'NONE',  ( 1.041036260628787957, 5.000000000000000888, -139.4530670678226443 ) ) ;
#9485 = CARTESIAN_POINT ( 'NONE',  ( -67.61300297071448995, 11.57753352799745450, -203.9033284969760302 ) ) ;
#9486 = CARTESIAN_POINT ( 'NONE',  ( -4.975935430107380597, -0.4889170748306866376, -1.000000000000011990 ) ) ;
#9487 = CARTESIAN_POINT ( 'NONE',  ( -1.346194077712559167, 3.937500000000001332, -6.749999999999999112 ) ) ;
#9488 = VECTOR ( 'NONE', #6185, 1000.000000000000227 ) ;
#9489 = CARTESIAN_POINT ( 'NONE',  ( 7.533261943714915532, 0.1450191290813469813, -105.4228757050405960 ) ) ;
#9490 = APPROVAL_ROLE ( '' ) ;
#9491 = EDGE_CURVE ( 'NONE', #9927, #8353, #6482, .T. ) ;
#9492 = CARTESIAN_POINT ( 'NONE',  ( -32.49979969806455671, 5.000000000000000888, -156.1716796081737186 ) ) ;
#9493 = CARTESIAN_POINT ( 'NONE',  ( -17.21625625355589762, 0.5158708274082715040, -130.3505683864442517 ) ) ;
#9494 = ORIENTED_EDGE ( 'NONE', *, *, #11100, .T. ) ;
#9495 = CARTESIAN_POINT ( 'NONE',  ( 5.149405770047748021, 1.500743523323658346, 3.597836686962641917 ) ) ;
#9496 = CARTESIAN_POINT ( 'NONE',  ( -2.298097038856278473, 3.125000000000000000, -1.201902961143720416 ) ) ;
#9497 = VECTOR ( 'NONE', #13764, 1000.000000000000000 ) ;
#9498 = CARTESIAN_POINT ( 'NONE',  ( -61.24268700632901385, 9.999999999999998224, -190.3758570956422886 ) ) ;
#9499 = CARTESIAN_POINT ( 'NONE',  ( 1.346194077712558057, 11.56249999999999822, -6.750000000000000000 ) ) ;
#9500 = CARTESIAN_POINT ( 'NONE',  ( 3.249999999999998224, 6.312500000000000000, -2.153805922287439945 ) ) ;
#9501 = ORIENTED_EDGE ( 'NONE', *, *, #219, .T. ) ;
#9502 = CARTESIAN_POINT ( 'NONE',  ( -2.850962077074172818, 15.00000000000000000, -123.0244887426839284 ) ) ;
#9503 = CARTESIAN_POINT ( 'NONE',  ( 26.64925767285982161, 4.000000000000000000, -138.6957041034480653 ) ) ;
#9504 = CARTESIAN_POINT ( 'NONE',  ( 10.25363971656158668, 14.55503923202592098, -106.4026536807294718 ) ) ;
#9505 = CARTESIAN_POINT ( 'NONE',  ( -1.346194077712559389, 2.062500000000000000, -0.2500000000000002220 ) ) ;
#9506 = CARTESIAN_POINT ( 'NONE',  ( -3.750000000000000000, 0.6875000000000000000, -1.946699141100893149 ) ) ;
#9507 = CARTESIAN_POINT ( 'NONE',  ( 3.750000000000000000, 3.750000000000000000, -3.500000000000000444 ) ) ;
#9508 = CARTESIAN_POINT ( 'NONE',  ( -0.2508417382212070335, 0.2913627682709560296, -7.146945437571385895 ) ) ;
#9509 = CARTESIAN_POINT ( 'NONE',  ( 0.000000000000000000, 6.500000000000000000, 0.2500000000000002220 ) ) ;
#9510 = CARTESIAN_POINT ( 'NONE',  ( 1.959483780728543234, 13.86208356520140583, 1.676081107764974654 ) ) ;
#9511 = CARTESIAN_POINT ( 'NONE',  ( -3.982786732524661755, 11.11191381569369696, -46.53277667289602704 ) ) ;
#9512 = EDGE_CURVE ( 'NONE', #11588, #12487, #6263, .T. ) ;
#9513 = ADVANCED_FACE ( 'NONE', ( #2785 ), #12432, .T. ) ;
#9514 = DIRECTION ( 'NONE',  ( 0.000000000000000000, 1.000000000000000000, 0.000000000000000000 ) ) ;
#9515 = EDGE_CURVE ( 'NONE', #14402, #5826, #594, .T. ) ;
#9516 = DIRECTION ( 'NONE',  ( -0.000000000000000000, -1.000000000000000000, -0.000000000000000000 ) ) ;
#9517 = CARTESIAN_POINT ( 'NONE',  ( 1.346194077712560944, 12.93750000000000000, -0.2500000000000010547 ) ) ;
#9518 = CARTESIAN_POINT ( 'NONE',  ( -9.240119717576693148, 10.34205777577377106, -104.6630069175297848 ) ) ;
#9519 = CARTESIAN_POINT ( 'NONE',  ( -64.71949702661652282, 14.00248011326570641, -198.7579215201884324 ) ) ;
#9520 = ORIENTED_EDGE ( 'NONE', *, *, #7320, .F. ) ;
#9521 = ORIENTED_EDGE ( 'NONE', *, *, #9246, .F. ) ;
#9522 = CARTESIAN_POINT ( 'NONE',  ( -2.633607816330602258, 4.336808689942017736E-16, -112.6800763249241015 ) ) ;
#9523 = FACE_OUTER_BOUND ( 'NONE', #3137, .T. ) ;
#9524 = CARTESIAN_POINT ( 'NONE',  ( -3.749999999999999556, 5.312500000000001776, -5.053300858899104853 ) ) ;
#9525 = CARTESIAN_POINT ( 'NONE',  ( 3.749999999999999112, 2.312500000000000000, -1.946699141100893149 ) ) ;
#9526 = CC_DESIGN_PERSON_AND_ORGANIZATION_ASSIGNMENT ( #8928, #12559, ( #1532 ) ) ;
#9527 = CARTESIAN_POINT ( 'NONE',  ( -0.4453226528549816265, -2.225540348348185052E-17, 2.000000000000000000 ) ) ;
#9528 = ORIENTED_EDGE ( 'NONE', *, *, #8813, .T. ) ;
#9529 = CARTESIAN_POINT ( 'NONE',  ( 3.249999999999998224, 5.312500000000000000, -2.153805922287439945 ) ) ;
#9530 = CARTESIAN_POINT ( 'NONE',  ( -51.27420002594509896, 15.00000000000000000, -153.1456608506698274 ) ) ;
#9531 = CARTESIAN_POINT ( 'NONE',  ( 4.074537004179775046, 8.673617379884034486E-16, -119.0111424115291356 ) ) ;
#9532 = CARTESIAN_POINT ( 'NONE',  ( 0.000000000000000000, 10.00000000000000000, -0.2500000000000002220 ) ) ;
#9533 = CARTESIAN_POINT ( 'NONE',  ( -4.876757625501888072, 15.00000000000000355, -115.1249378319107421 ) ) ;
#9534 = PERSON_AND_ORGANIZATION ( #2254, #6915 ) ;
#9535 = DIRECTION ( 'NONE',  ( 0.000000000000000000, 0.000000000000000000, -1.000000000000000000 ) ) ;
#9536 = CARTESIAN_POINT ( 'NONE',  ( 6.586989535938814200, 1.734723475976807094E-15, -124.5540024164598378 ) ) ;
#9537 = ORIENTED_EDGE ( 'NONE', *, *, #749, .T. ) ;
#9538 = CARTESIAN_POINT ( 'NONE',  ( -0.08788760335059413176, 15.00000000000000178, -112.5413916789569129 ) ) ;
#9539 = CARTESIAN_POINT ( 'NONE',  ( -25.11906781955738310, 0.000000000000000000, -198.9681998140721078 ) ) ;
#9540 = VERTEX_POINT ( 'NONE', #4103 ) ;
#9541 = ORIENTED_EDGE ( 'NONE', *, *, #11314, .F. ) ;
#9542 = CARTESIAN_POINT ( 'NONE',  ( -25.99849160774861900, 4.000000000000000000, -208.3968943305774815 ) ) ;
#9543 = CARTESIAN_POINT ( 'NONE',  ( -1.553300858899107073, 4.937500000000000888, -7.249999999999999112 ) ) ;
#9544 = CARTESIAN_POINT ( 'NONE',  ( 3.249999999999998224, 9.187500000000001776, -4.846194077712561388 ) ) ;
#9545 = ORIENTED_EDGE ( 'NONE', *, *, #5327, .F. ) ;
#9546 = CARTESIAN_POINT ( 'NONE',  ( 2.299001413603840138, 15.00000000000000000, -109.5170782816550030 ) ) ;
#9547 = CARTESIAN_POINT ( 'NONE',  ( 0.000000000000000000, 5.000000000000000000, -0.2500000000000002220 ) ) ;
#9548 = CARTESIAN_POINT ( 'NONE',  ( -6.764825266738188070, 1.389134033497039984E-16, -104.1458598414970993 ) ) ;
#9549 = CARTESIAN_POINT ( 'NONE',  ( 12.84147110302715511, 2.904872082602520944, -165.9573549719088135 ) ) ;
#9550 = APPLICATION_PROTOCOL_DEFINITION ( 'international standard', 'config_control_design', 1994, #2448 ) ;
#9551 = CARTESIAN_POINT ( 'NONE',  ( 0.03998412334521189021, 2.500000000000000444, 0.4529009045602680472 ) ) ;
#9552 = AXIS2_PLACEMENT_3D ( 'NONE', #7528, #7832, #11081 ) ;
#9553 = ORIENTED_EDGE ( 'NONE', *, *, #6501, .F. ) ;
#9554 = CARTESIAN_POINT ( 'NONE',  ( -0.9087754948914893438, 1.020558061026469510, -45.55632290616385660 ) ) ;
#9555 = CARTESIAN_POINT ( 'NONE',  ( 0.000000000000000000, 14.50000000000000355, 0.2499999999999998057 ) ) ;
#9556 = CARTESIAN_POINT ( 'NONE',  ( 26.71007981443199952, 5.000000000000000888, -136.8791680534710054 ) ) ;
#9557 = CARTESIAN_POINT ( 'NONE',  ( -64.02082625067613719, 12.73504901638480824, -210.7145675674813390 ) ) ;
#9558 = CARTESIAN_POINT ( 'NONE',  ( 3.434326385468031368E-15, 5.000000000000000000, -105.0258972447171857 ) ) ;
#9559 = CARTESIAN_POINT ( 'NONE',  ( -1.346194077712558945, 4.562500000000000000, -0.2500000000000002220 ) ) ;
#9560 = CARTESIAN_POINT ( 'NONE',  ( 10.02700419641868557, 1.638247714484150519, -106.0252156366010610 ) ) ;
#9561 = CALENDAR_DATE ( 2026, 8, 10 ) ;
#9562 = CARTESIAN_POINT ( 'NONE',  ( 3.249999999999998668, 14.68750000000000000, -4.846194077712560500 ) ) ;
#9563 = DIRECTION ( 'NONE',  ( 0.9982196940171963462, 0.000000000000000000, -0.05964429961207440289 ) ) ;
#9564 = ORIENTED_EDGE ( 'NONE', *, *, #979, .F. ) ;
#9565 = CARTESIAN_POINT ( 'NONE',  ( 4.078835579805053513, 0.1704923352145251980, -0.08935591895255695638 ) ) ;
#9566 = CARTESIAN_POINT ( 'NONE',  ( 3.249999999999998668, 2.687500000000000444, -4.846194077712560500 ) ) ;
#9567 = CARTESIAN_POINT ( 'NONE',  ( -66.90237725336980645, 10.00000000000000178, -173.2413874344579483 ) ) ;
#9568 = CARTESIAN_POINT ( 'NONE',  ( 1.346194077712560944, 12.93750000000000000, -0.2500000000000010547 ) ) ;
#9569 = CARTESIAN_POINT ( 'NONE',  ( -2.298097038856279362, 7.874999999999999112, -5.798097038856278473 ) ) ;
#9570 = ORIENTED_EDGE ( 'NONE', *, *, #534, .T. ) ;
#9571 = CARTESIAN_POINT ( 'NONE',  ( -6.078370696271480078, 9.999999999999998224, -118.0777554208214895 ) ) ;
#9572 = CARTESIAN_POINT ( 'NONE',  ( 3.834616502859925724, 14.88006226842800750, -1.031466025772356021 ) ) ;
#9573 = CARTESIAN_POINT ( 'NONE',  ( -15.11050069339551705, 15.00000000000000000, -146.5097068764709718 ) ) ;
#9574 = EDGE_CURVE ( 'NONE', #5270, #14745, #5277, .T. ) ;
#9575 = CARTESIAN_POINT ( 'NONE',  ( 2.298097038856278473, 0.6250000000000000000, -5.798097038856279362 ) ) ;
#9576 = CARTESIAN_POINT ( 'NONE',  ( -1.553300858899107073, 0.9375000000000000000, -7.249999999999999112 ) ) ;
#9577 = CARTESIAN_POINT ( 'NONE',  ( 2.651650429449553759, 5.875000000000000000, -0.8483495705504471296 ) ) ;
#9578 = CARTESIAN_POINT ( 'NONE',  ( 0.2625675448779695720, 5.000000000000000888, 2.974107436473219401 ) ) ;
#9579 = CARTESIAN_POINT ( 'NONE',  ( -1.553300858899107073, 5.937500000000002665, -7.249999999999999112 ) ) ;
#9580 = CARTESIAN_POINT ( 'NONE',  ( 4.871047274049744580, 14.73417332752070230, 0.4127525086329914550 ) ) ;
#9581 = FACE_OUTER_BOUND ( 'NONE', #4233, .T. ) ;
#9582 = CARTESIAN_POINT ( 'NONE',  ( 6.869258321017759350, 2.075239479414269450, -34.56909192082981974 ) ) ;
#9583 = CC_DESIGN_DATE_AND_TIME_ASSIGNMENT ( #12029, #9728, ( #13898 ) ) ;
#9584 = CARTESIAN_POINT ( 'NONE',  ( -1.224736468745108775, 5.434031181108818783E-13, -142.0096238726336821 ) ) ;
#9585 = CARTESIAN_POINT ( 'NONE',  ( 2.298097038856279362, 12.87500000000000178, -1.201902961143720860 ) ) ;
#9586 = CARTESIAN_POINT ( 'NONE',  ( 8.390458931657674313, 2.708951583600975876, 2.526057450858589792 ) ) ;
#9587 = CARTESIAN_POINT ( 'NONE',  ( -63.53877297815559189, 11.93648641405965627, -202.8585599469136298 ) ) ;
#9588 = ORIENTED_EDGE ( 'NONE', *, *, #10461, .T. ) ;
#9589 = CARTESIAN_POINT ( 'NONE',  ( 3.750000000000000000, 9.312500000000000000, -1.946699141100892705 ) ) ;
#9590 = ORIENTED_EDGE ( 'NONE', *, *, #7139, .T. ) ;
#9591 = CARTESIAN_POINT ( 'NONE',  ( -7.473411123654440047, 2.500000000000000444, -120.9918979907378969 ) ) ;
#9592 = CARTESIAN_POINT ( 'NONE',  ( -24.75251826597561333, 8.673617379884035472E-16, -198.2590867002109576 ) ) ;
#9593 = CARTESIAN_POINT ( 'NONE',  ( 3.749999999999999112, 8.812500000000000000, -1.946699141100892039 ) ) ;
#9594 = CARTESIAN_POINT ( 'NONE',  ( 2.651650429449553314, 2.375000000000000000, -0.8483495705504476847 ) ) ;
#9595 = DIRECTION ( 'NONE',  ( 0.000000000000000000, 0.000000000000000000, 1.000000000000000000 ) ) ;
#9596 = ORIENTED_EDGE ( 'NONE', *, *, #13782, .T. ) ;
#9597 = EDGE_CURVE ( 'NONE', #8123, #8666, #13436, .T. ) ;
#9598 = CARTESIAN_POINT ( 'NONE',  ( -5.534063745943522683, 0.09777223664412376669, -117.1292924427800415 ) ) ;
#9599 = CARTESIAN_POINT ( 'NONE',  ( 0.000000000000000000, 2.500000000000000000, -0.2500000000000002220 ) ) ;
#9600 = EDGE_CURVE ( 'NONE', #12872, #13945, #1820, .T. ) ;
#9601 = CARTESIAN_POINT ( 'NONE',  ( -70.02757949954413164, 15.00000000000000000, -189.2441461652899193 ) ) ;
#9602 = CARTESIAN_POINT ( 'NONE',  ( 3.460515205134051975, 8.673617379884035472E-16, -111.7394307393016391 ) ) ;
#9603 =( NAMED_UNIT ( * ) SI_UNIT ( $, .STERADIAN. ) SOLID_ANGLE_UNIT ( ) );
#9604 = CARTESIAN_POINT ( 'NONE',  ( 2.298097038856278473, 6.625000000000000000, -5.798097038856279362 ) ) ;
#9605 = PLANE ( 'NONE',  #14766 ) ;
#9606 = PERSON_AND_ORGANIZATION ( #428, #8643 ) ;
#9607 = CARTESIAN_POINT ( 'NONE',  ( -7.251835631655214165, 5.000000000000797584, -123.8995801872340223 ) ) ;
#9608 = DIRECTION ( 'NONE',  ( 0.000000000000000000, 0.000000000000000000, -1.000000000000000000 ) ) ;
#9609 = ORIENTED_EDGE ( 'NONE', *, *, #4980, .F. ) ;
#9610 = CARTESIAN_POINT ( 'NONE',  ( -0.3766621274091715987, 0.5000000000000000000, 0.1491815183709511716 ) ) ;
#9611 = LINE ( 'NONE', #12080, #12111 ) ;
#9612 = EDGE_LOOP ( 'NONE', ( #13483, #5953, #809, #2642 ) ) ;
#9613 = EDGE_LOOP ( 'NONE', ( #5299, #2061, #9775, #5488 ) ) ;
#9614 = CARTESIAN_POINT ( 'NONE',  ( 26.78844938926727437, 3.550418194419153739, -138.2511778740417299 ) ) ;
#9615 = CARTESIAN_POINT ( 'NONE',  ( -3.750000000000000000, 4.812500000000001776, -5.053300858899105741 ) ) ;
#9616 = CARTESIAN_POINT ( 'NONE',  ( -1.346194077712558945, 9.562500000000000000, -0.2500000000000002220 ) ) ;
#9617 = ORIENTED_EDGE ( 'NONE', *, *, #12990, .F. ) ;
#9618 = CARTESIAN_POINT ( 'NONE',  ( -4.445322652854981627, 5.288356561328269633E-16, 2.000000000000000000 ) ) ;
#9619 = CARTESIAN_POINT ( 'NONE',  ( -1.346194077712559389, 6.062500000000000000, -0.2500000000000002220 ) ) ;
#9620 = EDGE_CURVE ( 'NONE', #10989, #6383, #10205, .T. ) ;
#9621 = APPROVAL_PERSON_ORGANIZATION ( #6309, #11573, #1598 ) ;
#9622 = VECTOR ( 'NONE', #5652, 1000.000000000000000 ) ;
#9623 = CARTESIAN_POINT ( 'NONE',  ( -5.154409584717598136, 2.500000000000000888, -114.2587629972653360 ) ) ;
#9624 = CARTESIAN_POINT ( 'NONE',  ( 12.34479200262613396, 1.921688117712943011, -165.5931851613482593 ) ) ;
#9625 = CARTESIAN_POINT ( 'NONE',  ( -60.52034210924323787, 15.00000000000000178, -172.5548809364130705 ) ) ;
#9626 = DATE_TIME_ROLE ( 'creation_date' ) ;
#9627 = B_SPLINE_CURVE_WITH_KNOTS ( 'NONE', 3,
 ( #1701, #13620, #9974, #2795, #14713, #781, #4112, #3022, #3090, #11282, #12517, #8814, #10050, #7498, #13543, #7649, #10123, #5487 ),
 .UNSPECIFIED., .F., .F.,
 ( 4, 2, 2, 2, 2, 2, 2, 2, 4 ),
 ( -1.730026862698029293E-05, 0.002001214906283857280, 0.003010472493739274440, 0.003515101287466980418, 0.004019730081194686395, 0.005028987668650091412, 0.006038245256105494695, 0.007047502843560897977, 0.008056760431016302126 ),
 .UNSPECIFIED. ) ;
#9628 = CARTESIAN_POINT ( 'NONE',  ( 7.427446726622309647, 5.321094445766562764, -26.41501464507892294 ) ) ;
#9629 = CC_DESIGN_SECURITY_CLASSIFICATION ( #3971, ( #15318 ) ) ;
#9630 = VERTEX_POINT ( 'NONE', #8727 ) ;
#9631 = CARTESIAN_POINT ( 'NONE',  ( -2.298097038856278918, 1.375000000000000000, -5.798097038856277585 ) ) ;
#9632 = AXIS2_PLACEMENT_3D ( 'NONE', #8211, #3733, #12071 ) ;
#9633 = CARTESIAN_POINT ( 'NONE',  ( -2.237745678288944440, 15.00000000000000711, -122.9455479326446437 ) ) ;
#9634 = CARTESIAN_POINT ( 'NONE',  ( 1.553300858899105963, 14.06250000000000178, -7.249999999999999112 ) ) ;
#9635 = CIRCLE ( 'NONE', #25, 3.000000000000011990 ) ;
#9636 = CARTESIAN_POINT ( 'NONE',  ( -63.64301171304934002, 12.20966866758287850, -202.5945476619451142 ) ) ;
#9637 = CARTESIAN_POINT ( 'NONE',  ( 0.000000000000000000, 9.999999999999998224, -100.6237003951525537 ) ) ;
#9638 = CARTESIAN_POINT ( 'NONE',  ( -3.980102097228897738E-16, 3.000000000000000444, -6.749999999999999112 ) ) ;
#9639 = AXIS2_PLACEMENT_3D ( 'NONE', #4950, #2638, #12138 ) ;
#9640 = CARTESIAN_POINT ( 'NONE',  ( 9.627700091802285698, 1.251235758015203592, -106.1653571646377259 ) ) ;
#9641 = CIRCLE ( 'NONE', #12113, 5.000000000000010658 ) ;
#9642 = DATE_AND_TIME ( #528, #8698 ) ;
#9643 = AXIS2_PLACEMENT_3D ( 'NONE', #6853, #13818, #3145 ) ;
#9644 = FACE_OUTER_BOUND ( 'NONE', #1591, .T. ) ;
#9645 = DIRECTION ( 'NONE',  ( -0.000000000000000000, -0.000000000000000000, -1.000000000000000000 ) ) ;
#9646 = ORIENTED_EDGE ( 'NONE', *, *, #15104, .T. ) ;
#9647 = CARTESIAN_POINT ( 'NONE',  ( 4.510303310612941097, 0.6340196074359315537, 2.016023895169278379 ) ) ;
#9648 = CARTESIAN_POINT ( 'NONE',  ( 3.249999999999999112, 8.812500000000000000, -2.153805922287439945 ) ) ;
#9649 = CARTESIAN_POINT ( 'NONE',  ( -7.860067106259624126, 0.2490491084495508878, -104.5911971696796599 ) ) ;
#9650 = CARTESIAN_POINT ( 'NONE',  ( 2.298097038856279362, 13.87500000000000000, -1.201902961143720860 ) ) ;
#9651 = AXIS2_PLACEMENT_3D ( 'NONE', #1667, #14444, #10861 ) ;
#9652 = CARTESIAN_POINT ( 'NONE',  ( -2.298097038856278029, 7.625000000000001776, -1.201902961143720638 ) ) ;
#9653 = CARTESIAN_POINT ( 'NONE',  ( -6.078370696252020089, 15.00000000000000000, -118.0777554208285665 ) ) ;
#9654 = PLANE ( 'NONE',  #8987 ) ;
#9655 = CARTESIAN_POINT ( 'NONE',  ( 3.717577911061872520, 5.000000000000000888, -143.6771719914432595 ) ) ;
#9656 = CARTESIAN_POINT ( 'NONE',  ( -2.298097038856278918, 1.375000000000000000, -5.798097038856277585 ) ) ;
#9657 = CARTESIAN_POINT ( 'NONE',  ( -3.750000000000000000, 2.812500000000000444, -5.053300858899105741 ) ) ;
#9658 = CARTESIAN_POINT ( 'NONE',  ( 3.749999999999999112, 4.687500000000000888, -5.053300858899108405 ) ) ;
#9659 = CARTESIAN_POINT ( 'NONE',  ( -3.357934391919316308, 10.63007166822767680, -45.36073661948301350 ) ) ;
#9660 = CARTESIAN_POINT ( 'NONE',  ( 2.651650429449554203, 6.375000000000000888, -0.8483495705504471296 ) ) ;
#9661 = CARTESIAN_POINT ( 'NONE',  ( 4.619430714695810458, 14.36106363918124096, 1.856711022170560499 ) ) ;
#9662 = TOROIDAL_SURFACE ( 'NONE', #290, 9.499999999999941380, 2.500000000000000000 ) ;
#9663 = CARTESIAN_POINT ( 'NONE',  ( 9.068716941525980957, 1.734723475976807094E-15, -163.1923081219560174 ) ) ;
#9664 = ADVANCED_FACE ( 'NONE', ( #14776 ), #5477, .T. ) ;
#9665 = DIRECTION ( 'NONE',  ( -0.000000000000000000, -1.000000000000000000, -0.000000000000000000 ) ) ;
#9666 = EDGE_CURVE ( 'NONE', #2133, #10636, #11232, .T. ) ;
#9667 = PLANE ( 'NONE',  #12100 ) ;
#9668 = CARTESIAN_POINT ( 'NONE',  ( -15.50355452676521040, 8.673617379884035472E-16, -162.8135211086045899 ) ) ;
#9669 = CARTESIAN_POINT ( 'NONE',  ( -1.500000000000000000, 4.500000000000000888, 0.2500000000000002220 ) ) ;
#9670 = ORIENTED_EDGE ( 'NONE', *, *, #3850, .T. ) ;
#9671 = B_SPLINE_SURFACE_WITH_KNOTS ( 'NONE', 1, 3, ( 
 ( #10447, #7972, #14084, #2403, #4579, #11601, #10672, #11531, #1097, #15257, #9286, #7033, #14011, #945, #4727, #3337, #10370, #5870, #12846, #2259 ),
 ( #8045, #6965, #5802, #10524, #5649, #1023, #4648, #15108, #9357, #5728, #12773, #2180, #8195, #12926, #14165, #11747, #3568, #12999, #7101, #11820 ) ),
 .UNSPECIFIED., .F., .F., .F.,
 ( 2, 2 ),
 ( 4, 2, 2, 2, 2, 2, 2, 2, 2, 4 ),
 ( 0.000000000000000000, 1.000000000000000000 ),
 ( 0.1367849146739316402, 0.2678915559620899112, 0.3989981972502481544, 0.6612114798265646964, 0.9234247624028811829, 1.185638044979197669, 1.447851327555514267, 1.710064610131830642, 1.972277892708147018, 2.234491175284463615 ),
 .UNSPECIFIED. ) ;
#9672 = CARTESIAN_POINT ( 'NONE',  ( 1.553300858899109516, 8.437500000000000000, 0.2499999999999993616 ) ) ;
#9673 = ORIENTED_EDGE ( 'NONE', *, *, #8163, .T. ) ;
#9674 = CARTESIAN_POINT ( 'NONE',  ( -5.114912396279929219, 1.317715228986242930E-13, -113.5322278711262101 ) ) ;
#9675 = CARTESIAN_POINT ( 'NONE',  ( -23.43478651890449171, 8.673617379884035472E-16, -196.1076013386743853 ) ) ;
#9676 = CARTESIAN_POINT ( 'NONE',  ( -3.749999999999999556, 7.187500000000000000, -1.946699141100892927 ) ) ;
#9677 = CARTESIAN_POINT ( 'NONE',  ( 3.749999999999999112, 7.312500000000000000, -1.946699141100893149 ) ) ;
#9678 = CARTESIAN_POINT ( 'NONE',  ( -17.80444947669341360, 1.250643348872871874, -129.6916459345341650 ) ) ;
#9679 = EDGE_LOOP ( 'NONE', ( #7111, #3027 ) ) ;
#9680 = AXIS2_PLACEMENT_3D ( 'NONE', #2085, #8759, #5283 ) ;
#9681 = CARTESIAN_POINT ( 'NONE',  ( -6.822452048366741018, 0.5769591942652574357, -117.0063474466234084 ) ) ;
#9682 = CARTESIAN_POINT ( 'NONE',  ( 3.249999999999998224, 5.187499999999999112, -4.846194077712561388 ) ) ;
#9683 = CARTESIAN_POINT ( 'NONE',  ( -1.553300858899106629, 11.06250000000000000, 0.2500000000000002220 ) ) ;
#9684 = CARTESIAN_POINT ( 'NONE',  ( -64.33489900431855801, 14.99999999999999822, -199.0892663431833114 ) ) ;
#9685 = CARTESIAN_POINT ( 'NONE',  ( 5.760783416743275431, -1.035187345108135067E-30, -105.7086590657731904 ) ) ;
#9686 = CARTESIAN_POINT ( 'NONE',  ( 0.000000000000000000, 9.000000000000001776, -0.2500000000000002220 ) ) ;
#9687 = DIRECTION ( 'NONE',  ( 0.000000000000000000, -0.000000000000000000, 1.000000000000000000 ) ) ;
#9688 = APPROVAL_DATE_TIME ( #14574, #13108 ) ;
#9689 = LOCAL_TIME ( 12, 28, 20.00000000000000000, #10878 ) ;
#9690 = EDGE_CURVE ( 'NONE', #6819, #5529, #8719, .T. ) ;
#9691 = CARTESIAN_POINT ( 'NONE',  ( 4.950900406836953316, -4.336808689942017736E-15, -134.4284351762049141 ) ) ;
#9692 = CARTESIAN_POINT ( 'NONE',  ( 23.85593715806772153, 5.000000000000000888, -134.9913929663534873 ) ) ;
#9693 = VERTEX_POINT ( 'NONE', #10302 ) ;
#9694 = ADVANCED_FACE ( 'NONE', ( #1032 ), #1829, .T. ) ;
#9695 = CARTESIAN_POINT ( 'NONE',  ( -3.980102097228897245E-16, 13.50000000000000000, -6.749999999999999112 ) ) ;
#9696 = VERTEX_POINT ( 'NONE', #15266 ) ;
#9697 = LINE ( 'NONE', #3984, #8311 ) ;
#9698 = CARTESIAN_POINT ( 'NONE',  ( 21.23839455451635061, 4.156108327861118244E-16, -138.9326824654702648 ) ) ;
#9699 = CARTESIAN_POINT ( 'NONE',  ( 0.000000000000000000, 14.50000000000000355, 0.2499999999999998057 ) ) ;
#9700 = CIRCLE ( 'NONE', #11937, 0.9999999999999988898 ) ;
#9701 = CARTESIAN_POINT ( 'NONE',  ( -2.298097038856279362, 6.875000000000000000, -5.798097038856278473 ) ) ;
#9702 = CARTESIAN_POINT ( 'NONE',  ( 0.000000000000000000, 11.50000000000000000, -0.2500000000000002220 ) ) ;
#9703 = ORIENTED_EDGE ( 'NONE', *, *, #9600, .F. ) ;
#9704 = CARTESIAN_POINT ( 'NONE',  ( 0.000000000000000000, 1.750000000000000000, -1.771449424009386986 ) ) ;
#9705 = CARTESIAN_POINT ( 'NONE',  ( -1.346194077712559389, 5.062500000000001776, -0.2500000000000002220 ) ) ;
#9706 = APPROVAL ( #10842, 'UNKNOWN' ) ;
#9707 = CARTESIAN_POINT ( 'NONE',  ( -7.789898380477169759, 2.500000000000000888, -121.5509192307600586 ) ) ;
#9708 = CARTESIAN_POINT ( 'NONE',  ( -46.45656087453430416, 10.00000000000000000, -161.4072483220047047 ) ) ;
#9709 = CARTESIAN_POINT ( 'NONE',  ( -47.48189921986827500, 10.00000000000000000, -141.5723758807981483 ) ) ;
#9710 = AXIS2_PLACEMENT_3D ( 'NONE', #13443, #12023, #1675 ) ;
#9711 = PERSON_AND_ORGANIZATION ( #3176, #3020 ) ;
#9712 = EDGE_CURVE ( 'NONE', #9696, #2695, #9217, .T. ) ;
#9713 = CARTESIAN_POINT ( 'NONE',  ( -9.385448347264267355, 15.00000000000000000, -115.3551636530117150 ) ) ;
#9714 = EDGE_CURVE ( 'NONE', #7450, #1764, #15163, .T. ) ;
#9715 = EDGE_CURVE ( 'NONE', #5674, #13215, #10105, .T. ) ;
#9716 = VERTEX_POINT ( 'NONE', #3499 ) ;
#9717 = CARTESIAN_POINT ( 'NONE',  ( -1.346194077712559167, 13.93750000000000000, -6.749999999999999112 ) ) ;
#9718 = CARTESIAN_POINT ( 'NONE',  ( -3.750000000000000000, 13.25000000000000000, -3.499999999999999112 ) ) ;
#9719 = CARTESIAN_POINT ( 'NONE',  ( 9.044950117654433797, 6.000000000000000000, -141.4826476090360643 ) ) ;
#9720 = AXIS2_PLACEMENT_3D ( 'NONE', #14724, #13402, #9913 ) ;
#9721 = VECTOR ( 'NONE', #15181, 1000.000000000000000 ) ;
#9723 =( BOUNDED_CURVE ( )  B_SPLINE_CURVE ( 3, ( #1592, #11019, #792, #5496 ),
 .UNSPECIFIED., .F., .T. ) 
 B_SPLINE_CURVE_WITH_KNOTS ( ( 4, 4 ),
 ( 4.862919461057368054, 6.283185307179586232 ),
 .UNSPECIFIED. ) 
 CURVE ( )  GEOMETRIC_REPRESENTATION_ITEM ( )  RATIONAL_B_SPLINE_CURVE ( ( 1.000000000000000000, 0.8388501503673407855, 0.8388501503673407855, 1.000000000000000000 ) ) 
 REPRESENTATION_ITEM ( '' )  );
#9722 = CARTESIAN_POINT ( 'NONE',  ( -3.750000000000000000, 11.81250000000000178, -5.053300858899105741 ) ) ;
#9724 = CARTESIAN_POINT ( 'NONE',  ( -67.63300625564886559, 12.31334483152244452, -203.1194105661006404 ) ) ;
#9725 = DIRECTION ( 'NONE',  ( 0.000000000000000000, 1.000000000000000000, 0.000000000000000000 ) ) ;
#9726 = CARTESIAN_POINT ( 'NONE',  ( 1.346194077712558279, 4.062500000000001776, -6.750000000000000888 ) ) ;
#9727 = CARTESIAN_POINT ( 'NONE',  ( 7.868841884385653351, 0.2423173772081719524, -105.4238801664120047 ) ) ;
#9728 = DATE_TIME_ROLE ( 'classification_date' ) ;
#9729 = CARTESIAN_POINT ( 'NONE',  ( 0.000000000000000000, 15.00000000000000000, 0.2500000000000002220 ) ) ;
#9730 = AXIS2_PLACEMENT_3D ( 'NONE', #9813, #11048, #9091 ) ;
#9731 = FACE_OUTER_BOUND ( 'NONE', #14739, .T. ) ;
#9732 = AXIS2_PLACEMENT_3D ( 'NONE', #11014, #429, #8690 ) ;
#9733 = ORIENTED_EDGE ( 'NONE', *, *, #12014, .F. ) ;
#9734 = CARTESIAN_POINT ( 'NONE',  ( 4.402343282610404529, 0.5131405436234475204, 1.653012093462698617 ) ) ;
#9735 = CARTESIAN_POINT ( 'NONE',  ( 3.249999999999999556, 7.750000000000000000, -3.500000000000000000 ) ) ;
#9736 = CARTESIAN_POINT ( 'NONE',  ( -9.220836928148449019, 2.148733653916489406, -104.6587943809631156 ) ) ;
#9737 = CARTESIAN_POINT ( 'NONE',  ( -3.249999999999999556, 13.18749999999999822, -2.153805922287440833 ) ) ;
#9738 = CARTESIAN_POINT ( 'NONE',  ( -2.298097038856278029, 9.624999999999998224, -1.201902961143720638 ) ) ;
#9739 = DIRECTION ( 'NONE',  ( -1.000000000000000000, -0.000000000000000000, -0.000000000000000000 ) ) ;
#9740 = CARTESIAN_POINT ( 'NONE',  ( 0.5667764127758471160, 11.79980322240585622, 2.765452941203609072 ) ) ;
#9741 = CARTESIAN_POINT ( 'NONE',  ( -1.843872751587880776, 15.00000000000000000, -133.9216539038988003 ) ) ;
#9742 = CARTESIAN_POINT ( 'NONE',  ( 3.249999999999999112, 2.812500000000000000, -2.153805922287439945 ) ) ;
#9743 = AXIS2_PLACEMENT_3D ( 'NONE', #5747, #14261, #10611 ) ;
#9744 = CARTESIAN_POINT ( 'NONE',  ( -2.298097038856278029, 14.62500000000000178, -1.201902961143720638 ) ) ;
#9745 = CARTESIAN_POINT ( 'NONE',  ( 3.750000000000000000, 4.750000000000000000, -3.500000000000000444 ) ) ;
#9746 = CARTESIAN_POINT ( 'NONE',  ( -4.180890075922867766, 10.20972115200646257, -47.12409091164020936 ) ) ;
#9747 = CARTESIAN_POINT ( 'NONE',  ( -1.553300858899107073, 7.937500000000001776, -7.249999999999999112 ) ) ;
#9748 = CARTESIAN_POINT ( 'NONE',  ( 0.4077082524506932537, 11.25215624784117274, 2.875278165707306766 ) ) ;
#9749 = CARTESIAN_POINT ( 'NONE',  ( 11.27996230380671605, 0.9346580912078079617, -165.2299598695886971 ) ) ;
#9750 = CARTESIAN_POINT ( 'NONE',  ( 26.64925767285982161, 4.000000000000000000, -138.6957041034480653 ) ) ;
#9751 = CARTESIAN_POINT ( 'NONE',  ( 5.228075279701640099, 4.000000000000000000, -165.7939279834373849 ) ) ;
#9752 = DIRECTION ( 'NONE',  ( 0.000000000000000000, -1.000000000000000000, 0.000000000000000000 ) ) ;
#9753 = CARTESIAN_POINT ( 'NONE',  ( 5.228075279701640099, 1.000000000000000000, -167.7939279834373849 ) ) ;
#9754 = CARTESIAN_POINT ( 'NONE',  ( 11.44399236068192849, 4.000000000000000000, -138.9341978221715976 ) ) ;
#9755 = AXIS2_PLACEMENT_3D ( 'NONE', #6928, #913, #2149 ) ;
#9756 = VERTEX_POINT ( 'NONE', #3271 ) ;
#9757 = CARTESIAN_POINT ( 'NONE',  ( -4.592425496802573972E-16, 10.00000000000000000, -7.250000000000000000 ) ) ;
#9758 = EDGE_LOOP ( 'NONE', ( #14092, #3907, #93, #14719, #10845 ) ) ;
#9759 = CARTESIAN_POINT ( 'NONE',  ( -5.689254933302104966, 2.500000000000000444, -117.0567294044985829 ) ) ;
#9760 = CARTESIAN_POINT ( 'NONE',  ( -3.749999999999999556, 9.312499999999998224, -5.053300858899104853 ) ) ;
#9761 = CARTESIAN_POINT ( 'NONE',  ( -3.750000000000000000, 9.812500000000000000, -5.053300858899105741 ) ) ;
#9762 = DIRECTION ( 'NONE',  ( -0.000000000000000000, -1.000000000000000000, -0.000000000000000000 ) ) ;
#9763 = VERTEX_POINT ( 'NONE', #21 ) ;
#9764 = CARTESIAN_POINT ( 'NONE',  ( -3.249999999999999112, 4.687500000000000000, -2.153805922287440833 ) ) ;
#9765 = CARTESIAN_POINT ( 'NONE',  ( -2.651650429449552870, 9.125000000000000000, -0.8483495705504462414 ) ) ;
#9766 = CARTESIAN_POINT ( 'NONE',  ( -64.68844199977228016, 15.00000000000000000, -197.4748239606827553 ) ) ;
#9767 = LINE ( 'NONE', #1803, #14592 ) ;
#9768 = CARTESIAN_POINT ( 'NONE',  ( -1.346194077712559389, 8.062500000000000000, -0.2500000000000002220 ) ) ;
#9769 = DATE_AND_TIME ( #3736, #8385 ) ;
#9770 = CARTESIAN_POINT ( 'NONE',  ( 0.6300320263538776722, -4.336808689942017736E-15, -128.5410338263872632 ) ) ;
#9771 = LINE ( 'NONE', #12241, #12091 ) ;
#9772 = ORIENTED_EDGE ( 'NONE', *, *, #2239, .F. ) ;
#9773 = DIRECTION ( 'NONE',  ( 0.000000000000000000, 0.000000000000000000, -1.000000000000000000 ) ) ;
#9774 = LINE ( 'NONE', #4065, #6413 ) ;
#9775 = ORIENTED_EDGE ( 'NONE', *, *, #12239, .F. ) ;
#9776 = VERTEX_POINT ( 'NONE', #11613 ) ;
#9777 = DIRECTION ( 'NONE',  ( -0.000000000000000000, -1.000000000000000000, -0.000000000000000000 ) ) ;
#9778 = CARTESIAN_POINT ( 'NONE',  ( 3.749999999999999556, 11.25000000000000178, -3.500000000000000444 ) ) ;
#9779 = CARTESIAN_POINT ( 'NONE',  ( 3.249999999999998224, 13.18750000000000000, -4.846194077712561388 ) ) ;
#9780 = CARTESIAN_POINT ( 'NONE',  ( 1.346194077712561166, 9.437500000000000000, -0.2500000000000011102 ) ) ;
#9781 = ADVANCED_FACE ( 'NONE', ( #11466 ), #3533, .T. ) ;
#9782 = ORIENTED_EDGE ( 'NONE', *, *, #11502, .F. ) ;
#9783 = LINE ( 'NONE', #8457, #2314 ) ;
#9784 = CARTESIAN_POINT ( 'NONE',  ( 0.000000000000000000, 6.000000000000000000, -0.2500000000000002220 ) ) ;
#9785 = EDGE_CURVE ( 'NONE', #10699, #922, #11763, .T. ) ;
#9786 = B_SPLINE_CURVE_WITH_KNOTS ( 'NONE', 3,
 ( #2828, #9698, #7529, #192, #13340, #14431, #8529, #12314, #8769, #13501, #12083, #4902, #1507, #13184, #13263, #269, #9614, #12004, #14583, #2748 ),
 .UNSPECIFIED., .F., .F.,
 ( 4, 2, 2, 2, 2, 2, 2, 2, 2, 4 ),
 ( -1.419797821985954122E-05, 0.001094435061963930454, 0.002203068102147720704, 0.003311701142331510955, 0.004420334182515300338, 0.005528967222699090155, 0.006083283742790985930, 0.006637600262882880839, 0.007746233303066660247, 0.008854866343250441391 ),
 .UNSPECIFIED. ) ;
#9787 = CARTESIAN_POINT ( 'NONE',  ( -5.511151914899733661, 2.500000000000000000, -116.3187303629814551 ) ) ;
#9788 = CARTESIAN_POINT ( 'NONE',  ( -59.56434992273744200, 9.999999999999994671, -183.8842187088368121 ) ) ;
#9789 = DIRECTION ( 'NONE',  ( 1.000000000000000000, 0.000000000000000000, 0.000000000000000000 ) ) ;
#9790 = PERSON_AND_ORGANIZATION ( #3176, #3020 ) ;
#9791 = DIRECTION ( 'NONE',  ( -0.9961255586397049777, -0.000000000000000000, 0.08794243244723005948 ) ) ;
#9792 = ORIENTED_EDGE ( 'NONE', *, *, #14897, .T. ) ;
#9793 = CARTESIAN_POINT ( 'NONE',  ( 3.249999999999999112, 9.812500000000000000, -2.153805922287439945 ) ) ;
#9794 = CARTESIAN_POINT ( 'NONE',  ( 1.346194077712558279, 14.06250000000000178, -6.750000000000000888 ) ) ;
#9795 = CARTESIAN_POINT ( 'NONE',  ( -3.750000000000000000, 14.25000000000000000, -3.499999999999999112 ) ) ;
#9796 = CARTESIAN_POINT ( 'NONE',  ( -2.923188566258836385, 1.750000000000027756, 0.7596801491339106871 ) ) ;
#9797 = CARTESIAN_POINT ( 'NONE',  ( 3.749999999999999112, 3.812500000000000000, -1.946699141100892039 ) ) ;
#9798 = EDGE_CURVE ( 'NONE', #5990, #5060, #10830, .T. ) ;
#9799 = CARTESIAN_POINT ( 'NONE',  ( -64.96615686214629193, 15.33131988198272744, -206.4716339831645087 ) ) ;
#9800 = DIRECTION ( 'NONE',  ( -0.02181900108494737658, 0.000000000000000000, 0.9997619372588931741 ) ) ;
#9801 = CARTESIAN_POINT ( 'NONE',  ( 8.641297968024963083, 0.6305609033237062899, -105.9901394978445097 ) ) ;
#9802 = CALENDAR_DATE ( 2026, 8, 10 ) ;
#9803 = DIRECTION ( 'NONE',  ( 0.000000000000000000, -1.000000000000000000, 0.000000000000000000 ) ) ;
#9804 = LINE ( 'NONE', #10964, #3977 ) ;
#9805 = VERTEX_POINT ( 'NONE', #12065 ) ;
#9806 = CARTESIAN_POINT ( 'NONE',  ( 4.999884908349637946, 0.09438068890030250346, -1.653151978968653957 ) ) ;
#9807 = CARTESIAN_POINT ( 'NONE',  ( 1.346194077712560944, 5.937500000000000000, -0.2500000000000011102 ) ) ;
#9808 = CARTESIAN_POINT ( 'NONE',  ( -48.59171165233305345, 9.999999999999998224, -142.5285849061865804 ) ) ;
#9809 = CARTESIAN_POINT ( 'NONE',  ( -3.249999999999999556, 14.18750000000000000, -2.153805922287440833 ) ) ;
#9810 = CARTESIAN_POINT ( 'NONE',  ( -3.249999999999999112, 9.812500000000000000, -4.846194077712558723 ) ) ;
#9811 = DIRECTION ( 'NONE',  ( 0.9939692226109179130, 0.000000000000000000, -0.1096594022519158801 ) ) ;
#9812 = SHAPE_REPRESENTATION ( 'Nut_Predeterminado', ( #9419 ), #1768 ) ;
#9813 = CARTESIAN_POINT ( 'NONE',  ( 30.32986759126112730, 0.7500000000000000000, 43.04214087805580391 ) ) ;
#9814 = CARTESIAN_POINT ( 'NONE',  ( 11.04730216892670569, 12.84598696159166487, -107.1178495030794693 ) ) ;
#9815 = CARTESIAN_POINT ( 'NONE',  ( 1.346194077712560944, 5.937500000000000000, -0.2500000000000010547 ) ) ;
#9816 = CARTESIAN_POINT ( 'NONE',  ( 3.749999999999998668, 3.187500000000000444, -5.053300858899108405 ) ) ;
#9817 = ADVANCED_FACE ( 'NONE', ( #10759 ), #9834, .T. ) ;
#9818 = CARTESIAN_POINT ( 'NONE',  ( 0.000000000000000000, 10.00000000000000000, 0.2500000000000002220 ) ) ;
#9819 = CARTESIAN_POINT ( 'NONE',  ( 0.09756493787362907621, 2.578155857656784455, 1.105119855559491437 ) ) ;
#9820 = CARTESIAN_POINT ( 'NONE',  ( 2.651650429449554203, 7.375000000000000000, -0.8483495705504471296 ) ) ;
#9821 = CARTESIAN_POINT ( 'NONE',  ( 4.913233174174957085, 14.82748211479344747, -0.2684095748386393088 ) ) ;
#9822 = CARTESIAN_POINT ( 'NONE',  ( 12.90827548330815766, 3.452651285030396977, -166.3555584590855858 ) ) ;
#9823 = DIRECTION ( 'NONE',  ( 1.000000000000000000, 0.000000000000000000, 0.000000000000000000 ) ) ;
#9824 = CARTESIAN_POINT ( 'NONE',  ( -1.331179381611672374, 8.673617379884035472E-16, -147.1845506124080032 ) ) ;
#9825 = CARTESIAN_POINT ( 'NONE',  ( -25.82983890416511841, 5.000000000000000000, -142.4527639562402328 ) ) ;
#9826 = CARTESIAN_POINT ( 'NONE',  ( 8.306309981135230558, 2.550729144823657979, 2.473100317603431186 ) ) ;
#9827 = ORIENTED_EDGE ( 'NONE', *, *, #7409, .F. ) ;
#9828 = CARTESIAN_POINT ( 'NONE',  ( 1.346194077712561166, 0.4375000000000000555, -0.2500000000000011102 ) ) ;
#9829 = ORIENTED_EDGE ( 'NONE', *, *, #8181, .T. ) ;
#9830 = DIRECTION ( 'NONE',  ( 0.000000000000000000, 1.000000000000000000, 0.000000000000000000 ) ) ;
#9831 = CARTESIAN_POINT ( 'NONE',  ( 4.716951098700676859, -2.490287375297126626, -44.10818225254241298 ) ) ;
#9832 = CARTESIAN_POINT ( 'NONE',  ( -1.553300858899107295, 8.437500000000000000, -7.250000000000000000 ) ) ;
#9833 = CARTESIAN_POINT ( 'NONE',  ( -4.592425496802573972E-16, 8.999999999999998224, -7.250000000000000000 ) ) ;
#9834 = CYLINDRICAL_SURFACE ( 'NONE', #8470, 2.000000000000000000 ) ;
#9835 = ORIENTED_EDGE ( 'NONE', *, *, #10998, .T. ) ;
#9836 = CARTESIAN_POINT ( 'NONE',  ( 3.249999999999998224, 4.187500000000000888, -4.846194077712561388 ) ) ;
#9837 = CARTESIAN_POINT ( 'NONE',  ( -1.553300858899106629, 8.062500000000000000, 0.2500000000000002220 ) ) ;
#9838 = CARTESIAN_POINT ( 'NONE',  ( -65.10000466134623309, 15.00000000000000000, -191.5398038754765935 ) ) ;
#9839 = CARTESIAN_POINT ( 'NONE',  ( 8.475206276408092876, 0.000000000000000000, -34.56909192082981974 ) ) ;
#9840 = COORDINATED_UNIVERSAL_TIME_OFFSET ( 0, 0, .AHEAD. ) ;
#9841 = CARTESIAN_POINT ( 'NONE',  ( -3.249999999999999556, 8.250000000000000000, -3.499999999999999556 ) ) ;
#9842 = CARTESIAN_POINT ( 'NONE',  ( -3.846760974179296966, 15.00000000000000355, -118.7367476769033345 ) ) ;
#9843 = CARTESIAN_POINT ( 'NONE',  ( -7.626890066815782632, 5.000000000000794032, -122.9684017742212632 ) ) ;
#9844 = CARTESIAN_POINT ( 'NONE',  ( 7.148068729939693000, 2.490287375297123962, -34.56909192082981974 ) ) ;
#9845 = VERTEX_POINT ( 'NONE', #7430 ) ;
#9846 = CARTESIAN_POINT ( 'NONE',  ( -4.090890948359609425, 15.00000000000000000, -103.1929727064838289 ) ) ;
#9847 = DIRECTION ( 'NONE',  ( -0.8674617751425300893, 0.000000000000000000, -0.4975038378410468476 ) ) ;
#9848 = ORIENTED_EDGE ( 'NONE', *, *, #6268, .F. ) ;
#9849 = ORIENTED_EDGE ( 'NONE', *, *, #7231, .F. ) ;
#9850 = CARTESIAN_POINT ( 'NONE',  ( 1.500000000000000000, 5.000000000000000000, -0.2499999999999997780 ) ) ;
#9851 = CARTESIAN_POINT ( 'NONE',  ( -1.553300858899106629, 13.56250000000000000, 0.2499999999999998335 ) ) ;
#9852 = CARTESIAN_POINT ( 'NONE',  ( -1.346194077712559167, 11.93750000000000178, -6.749999999999999112 ) ) ;
#9853 = CARTESIAN_POINT ( 'NONE',  ( -3.249999999999999556, 11.75000000000000178, -3.500000000000000000 ) ) ;
#9854 = ORIENTED_EDGE ( 'NONE', *, *, #14917, .F. ) ;
#9855 = CARTESIAN_POINT ( 'NONE',  ( -37.86885108244810283, 9.999999999999998224, -139.8897182464016566 ) ) ;
#9856 = CARTESIAN_POINT ( 'NONE',  ( 2.298097038856278473, 8.625000000000000000, -5.798097038856279362 ) ) ;
#9857 = DIRECTION ( 'NONE',  ( 0.7779936141972744190, 0.000000000000000000, 0.6282721832679388774 ) ) ;
#9858 =( REPRESENTATION_RELATIONSHIP ('NONE','NONE', #11394, #4394 ) REPRESENTATION_RELATIONSHIP_WITH_TRANSFORMATION ( #3899 )SHAPE_REPRESENTATION_RELATIONSHIP( ) );
#9859 = CARTESIAN_POINT ( 'NONE',  ( 13.34352170149614025, 13.85492800443912387, -126.0862001755899371 ) ) ;
#9860 = DIRECTION ( 'NONE',  ( 0.000000000000000000, 0.000000000000000000, 1.000000000000000000 ) ) ;
#9861 = CARTESIAN_POINT ( 'NONE',  ( -66.44604053271804389, 5.000000000000000888, -157.9117883361228394 ) ) ;
#9862 = APPROVAL_DATE_TIME ( #2444, #12267 ) ;
#9863 = DIRECTION ( 'NONE',  ( 0.000000000000000000, 1.000000000000000000, 0.000000000000000000 ) ) ;
#9864 = VERTEX_POINT ( 'NONE', #6280 ) ;
#9865 = EDGE_CURVE ( 'NONE', #13794, #1404, #10994, .T. ) ;
#9866 = CARTESIAN_POINT ( 'NONE',  ( -1.346194077712558945, 13.56250000000000000, -0.2500000000000002220 ) ) ;
#9867 = CARTESIAN_POINT ( 'NONE',  ( -4.592425496802573972E-16, 13.50000000000000000, -7.249999999999999112 ) ) ;
#9868 = VERTEX_POINT ( 'NONE', #4812 ) ;
#9869 = APPROVAL_PERSON_ORGANIZATION ( #12655, #15090, #13746 ) ;
#9870 = DIRECTION ( 'NONE',  ( -1.000000000000000000, -0.000000000000000000, -0.000000000000000000 ) ) ;
#9871 = AXIS2_PLACEMENT_3D ( 'NONE', #8792, #13522, #13742 ) ;
#9872 = CARTESIAN_POINT ( 'NONE',  ( -3.750000000000000000, 1.250000000000000000, -3.499999999999999112 ) ) ;
#9873 = CARTESIAN_POINT ( 'NONE',  ( -49.26721305452313260, 5.000000000000000888, -156.1716796081737471 ) ) ;
#9874 = CARTESIAN_POINT ( 'NONE',  ( -4.507463604512252253, 5.000000000000000000, -2.585105772303598393 ) ) ;
#9875 = CARTESIAN_POINT ( 'NONE',  ( 11.29096412601620258, 4.293855562754802513, -106.8042879785164274 ) ) ;
#9876 = PERSON_AND_ORGANIZATION_ROLE ( 'classification_officer' ) ;
#9877 = CARTESIAN_POINT ( 'NONE',  ( -2.837468109123920446, 2.529993217055223287, -0.7946808062301191633 ) ) ;
#9878 = FACE_OUTER_BOUND ( 'NONE', #11042, .T. ) ;
#9879 = AXIS2_PLACEMENT_3D ( 'NONE', #12691, #6590, #11299 ) ;
#9880 = VERTEX_POINT ( 'NONE', #2414 ) ;
#9881 = CARTESIAN_POINT ( 'NONE',  ( 1.346194077712558279, 6.562500000000000000, -6.750000000000000000 ) ) ;
#9882 = CARTESIAN_POINT ( 'NONE',  ( -9.108435135009571582, 1.571332947940224045, -105.1067939785190219 ) ) ;
#9883 = CARTESIAN_POINT ( 'NONE',  ( -3.980102097228897245E-16, 13.50000000000000000, -6.749999999999999112 ) ) ;
#9884 = CARTESIAN_POINT ( 'NONE',  ( 3.249999999999999556, 12.25000000000000000, -3.500000000000000000 ) ) ;
#9885 = CARTESIAN_POINT ( 'NONE',  ( -8.241439964468746382, 15.00000000000000888, -106.0832790697330239 ) ) ;
#9886 = DIRECTION ( 'NONE',  ( 0.000000000000000000, 1.000000000000000000, 0.000000000000000000 ) ) ;
#9887 = VECTOR ( 'NONE', #4729, 1000.000000000000114 ) ;
#9888 = DIRECTION ( 'NONE',  ( 0.05964429961207241837, 0.000000000000000000, 0.9982196940171965682 ) ) ;
#9889 = CARTESIAN_POINT ( 'NONE',  ( -3.980102097228897245E-16, 6.500000000000000888, -6.749999999999999112 ) ) ;
#9890 = CARTESIAN_POINT ( 'NONE',  ( 3.749999999999999112, 7.312500000000000000, -1.946699141100893149 ) ) ;
#9891 = AXIS2_PLACEMENT_3D ( 'NONE', #4843, #13432, #3611 ) ;
#9892 = VECTOR ( 'NONE', #12116, 1000.000000000000000 ) ;
#9893 = CARTESIAN_POINT ( 'NONE',  ( -4.592425496802573972E-16, 7.500000000000000000, -7.249999999999999112 ) ) ;
#9894 = CARTESIAN_POINT ( 'NONE',  ( -4.119321715443209797, 10.47408532934288772, -46.53149779072169423 ) ) ;
#9895 = CARTESIAN_POINT ( 'NONE',  ( -3.750000000000000000, 10.81250000000000000, -5.053300858899105741 ) ) ;
#9896 = CARTESIAN_POINT ( 'NONE',  ( 1.078231930479278899, 6.000000000000000000, -139.4303258909232852 ) ) ;
#9897 = CARTESIAN_POINT ( 'NONE',  ( -0.5793326530874193248, -2.529993217055220178, -43.47630266472464911 ) ) ;
#9898 = DIRECTION ( 'NONE',  ( -0.9961255586397050887, 0.000000000000000000, 0.08794243244723005948 ) ) ;
#9899 = CIRCLE ( 'NONE', #15105, 5.000000000000000000 ) ;
#9900 = DIRECTION ( 'NONE',  ( 0.000000000000000000, 0.000000000000000000, 1.000000000000000000 ) ) ;
#9901 = CARTESIAN_POINT ( 'NONE',  ( -0.3766621274091710991, 0.2295137623791638215, -7.070595193497560160 ) ) ;
#9902 = AXIS2_PLACEMENT_3D ( 'NONE', #4977, #9464, #8295 ) ;
#9903 =( BOUNDED_CURVE ( )  B_SPLINE_CURVE ( 3, ( #8020, #2157, #15156, #3382 ),
 .UNSPECIFIED., .F., .T. ) 
 B_SPLINE_CURVE_WITH_KNOTS ( ( 4, 4 ),
 ( 0.000000000000000000, 0.1427305759106287653 ),
 .UNSPECIFIED. ) 
 CURVE ( )  GEOMETRIC_REPRESENTATION_ITEM ( )  RATIONAL_B_SPLINE_CURVE ( ( 1.000000000000000000, 0.9983030522886272573, 0.9983030522886272573, 1.000000000000000000 ) ) 
 REPRESENTATION_ITEM ( '' )  );
#9904 = AXIS2_PLACEMENT_3D ( 'NONE', #9991, #12612, #2886 ) ;
#9905 = EDGE_CURVE ( 'NONE', #3117, #5060, #6979, .T. ) ;
#9906 = CARTESIAN_POINT ( 'NONE',  ( 0.2499999999999999445, 4.500000000000000888, 1.500000000000000222 ) ) ;
#9907 = CARTESIAN_POINT ( 'NONE',  ( -1.553300858899107073, 12.93750000000000178, -7.249999999999999112 ) ) ;
#9908 = VERTEX_POINT ( 'NONE', #5119 ) ;
#9909 = LINE ( 'NONE', #14643, #2296 ) ;
#9910 = CARTESIAN_POINT ( 'NONE',  ( 8.978461304436876844, -1.921202954650397476, -40.45944830867332342 ) ) ;
#9911 = CARTESIAN_POINT ( 'NONE',  ( -4.592425496802573972E-16, 8.500000000000000000, -7.249999999999999112 ) ) ;
#9912 = CARTESIAN_POINT ( 'NONE',  ( 3.749999999999998668, 9.187500000000001776, -5.053300858899108405 ) ) ;
#9913 = DIRECTION ( 'NONE',  ( -0.02181900108494679719, 0.000000000000000000, 0.9997619372588931741 ) ) ;
#9914 = ORIENTED_EDGE ( 'NONE', *, *, #7214, .T. ) ;
#9915 =( BOUNDED_CURVE ( )  B_SPLINE_CURVE ( 3, ( #14555, #14637, #11057, #6570 ),
 .UNSPECIFIED., .F., .F. ) 
 B_SPLINE_CURVE_WITH_KNOTS ( ( 4, 4 ),
 ( 0.3190780441241196641, 2.822514609465673452 ),
 .UNSPECIFIED. ) 
 CURVE ( )  GEOMETRIC_REPRESENTATION_ITEM ( )  RATIONAL_B_SPLINE_CURVE ( ( 1.000000000000000000, 0.5424608492517398739, 0.5424608492517398739, 1.000000000000000000 ) ) 
 REPRESENTATION_ITEM ( '' )  );
#9916 = CARTESIAN_POINT ( 'NONE',  ( -3.249999999999999112, 8.687500000000003553, -2.153805922287440833 ) ) ;
#9917 = CARTESIAN_POINT ( 'NONE',  ( -2.651650429449553314, 8.375000000000000000, -6.151650429449552426 ) ) ;
#9918 = CARTESIAN_POINT ( 'NONE',  ( -70.04737159589244300, 9.999999999999998224, -194.4639900966930099 ) ) ;
#9919 = B_SPLINE_CURVE_WITH_KNOTS ( 'NONE', 3,
 ( #564, #14798, #5275, #5200, #8973, #4193, #7814, #8900, #12526, #13552, #8671, #12300, #3030, #13704, #485, #4124, #10133, #8825 ),
 .UNSPECIFIED., .F., .F.,
 ( 4, 2, 2, 2, 2, 2, 2, 2, 4 ),
 ( 0.000000000000000000, 0.0006487559250799439540, 0.001297511850159887908, 0.001946267775239831754, 0.002595023700319775816, 0.003243779625399719879, 0.003892535550479663507, 0.004541291475559607570, 0.005190047400639551632 ),
 .UNSPECIFIED. ) ;
#9920 = CARTESIAN_POINT ( 'NONE',  ( 3.158384440324541131, 0.000000000000000000, -1.000000000000028644 ) ) ;
#9921 = CARTESIAN_POINT ( 'NONE',  ( -1.346194077712559389, 10.43750000000000000, -6.749999999999999112 ) ) ;
#9922 = CARTESIAN_POINT ( 'NONE',  ( -7.068384139542111200, 10.00000000000000355, -107.3966098791943864 ) ) ;
#9923 = CARTESIAN_POINT ( 'NONE',  ( -3.149239014469442210, 5.000000000000002665, -131.9551168572792790 ) ) ;
#9924 = CARTESIAN_POINT ( 'NONE',  ( 9.247146435752135574, 5.000000000000000888, -109.6962599557244715 ) ) ;
#9925 = CARTESIAN_POINT ( 'NONE',  ( 0.3766621274091715987, 0.2956834184403337451, -6.863050255469942407 ) ) ;
#9926 = AXIS2_PLACEMENT_3D ( 'NONE', #7767, #12481, #4296 ) ;
#9927 = VERTEX_POINT ( 'NONE', #7352 ) ;
#9928 = CARTESIAN_POINT ( 'NONE',  ( 8.935548306746156300, 9.999999999999998224, 2.855381328098127725 ) ) ;
#9929 = CARTESIAN_POINT ( 'NONE',  ( -0.1260668993691365092, 0.2851798274189282778, -6.863050255469941519 ) ) ;
#9930 = CARTESIAN_POINT ( 'NONE',  ( 0.000000000000000000, 12.50000000000000178, 0.2499999999999998057 ) ) ;
#9931 = CARTESIAN_POINT ( 'NONE',  ( -2.298097038856278029, 10.62500000000000178, -1.201902961143720638 ) ) ;
#9932 = CARTESIAN_POINT ( 'NONE',  ( 3.249999999999998224, 13.31250000000000178, -2.153805922287439945 ) ) ;
#9933 = VERTEX_POINT ( 'NONE', #10682 ) ;
#9934 = CARTESIAN_POINT ( 'NONE',  ( -3.980102097228897245E-16, 7.500000000000000000, -6.749999999999999112 ) ) ;
#9935 = CARTESIAN_POINT ( 'NONE',  ( -6.288157641191917335, 13.40945642053105225, -124.9981450708252595 ) ) ;
#9936 = APPROVAL_PERSON_ORGANIZATION ( #11657, #2654, #1213 ) ;
#9937 = CARTESIAN_POINT ( 'NONE',  ( 9.998507851868444263, 12.56623780283944924, -45.85017076944640735 ) ) ;
#9938 = CARTESIAN_POINT ( 'NONE',  ( 6.085378087782216561, 4.179870625069618484, 5.225355098807171750 ) ) ;
#9939 = CARTESIAN_POINT ( 'NONE',  ( -0.4453226528549816265, -2.225540348348185052E-17, -1.000000000000000000 ) ) ;
#9940 = PERSON_AND_ORGANIZATION ( #3176, #3020 ) ;
#9941 = DIRECTION ( 'NONE',  ( 0.000000000000000000, 0.000000000000000000, -1.000000000000000000 ) ) ;
#9942 = ORIENTED_EDGE ( 'NONE', *, *, #1644, .T. ) ;
#9943 = CARTESIAN_POINT ( 'NONE',  ( 0.000000000000000000, 14.50000000000000000, -0.2500000000000002220 ) ) ;
#9944 = CARTESIAN_POINT ( 'NONE',  ( 1.553300858899105963, 13.56250000000000000, -7.250000000000000888 ) ) ;
#9945 = ORIENTED_EDGE ( 'NONE', *, *, #9130, .F. ) ;
#9946 = FACE_OUTER_BOUND ( 'NONE', #7213, .T. ) ;
#9947 = CARTESIAN_POINT ( 'NONE',  ( -2.651650429449552870, 2.125000000000000000, -0.8483495705504462414 ) ) ;
#9948 = AXIS2_PLACEMENT_3D ( 'NONE', #13824, #3226, #2077 ) ;
#9949 = FACE_OUTER_BOUND ( 'NONE', #14192, .T. ) ;
#9950 = CARTESIAN_POINT ( 'NONE',  ( 0.2677563320781928824, 0.4815089180969744365, 3.032880925044830978 ) ) ;
#9951 = CARTESIAN_POINT ( 'NONE',  ( -4.592425496802573972E-16, 2.500000000000000000, -7.249999999999999112 ) ) ;
#9952 = PERSON_AND_ORGANIZATION ( #3176, #3020 ) ;
#9953 = CARTESIAN_POINT ( 'NONE',  ( -67.35192000380439481, 14.27092917653249238, -197.4726913168000237 ) ) ;
#9954 = FACE_OUTER_BOUND ( 'NONE', #968, .T. ) ;
#9955 = ORIENTED_EDGE ( 'NONE', *, *, #14342, .F. ) ;
#9956 = CARTESIAN_POINT ( 'NONE',  ( 3.249999999999998668, 7.687500000000000000, -4.846194077712560500 ) ) ;
#9957 = CIRCLE ( 'NONE', #6998, 0.5000000000000018874 ) ;
#9958 = CARTESIAN_POINT ( 'NONE',  ( -4.018470066652908734, 7.379999999999995453, -45.51728475810764962 ) ) ;
#9959 = AXIS2_PLACEMENT_3D ( 'NONE', #12750, #11656, #8098 ) ;
#9960 = CARTESIAN_POINT ( 'NONE',  ( 2.298097038856278029, 4.125000000000000000, -5.798097038856279362 ) ) ;
#9961 = CARTESIAN_POINT ( 'NONE',  ( -1.346194077712558945, 9.562500000000000000, -0.2500000000000002220 ) ) ;
#9962 = DIRECTION ( 'NONE',  ( 0.000000000000000000, 0.000000000000000000, -1.000000000000000000 ) ) ;
#9963 = CARTESIAN_POINT ( 'NONE',  ( -9.623069100187665370, 4.336808689942017736E-16, -128.0716982634005774 ) ) ;
#9964 = CARTESIAN_POINT ( 'NONE',  ( -2.298097038856278473, 3.125000000000000000, -1.201902961143720416 ) ) ;
#9965 = CARTESIAN_POINT ( 'NONE',  ( 1.553300858899105963, 4.062500000000001776, -7.249999999999999112 ) ) ;
#9966 = CARTESIAN_POINT ( 'NONE',  ( -3.750000000000000000, 11.18750000000000000, -1.946699141100892927 ) ) ;
#9967 = EDGE_CURVE ( 'NONE', #6060, #15209, #13247, .T. ) ;
#9968 = CARTESIAN_POINT ( 'NONE',  ( -9.385448347264267355, 5.000000000000000888, -115.3551636530117150 ) ) ;
#9969 = CARTESIAN_POINT ( 'NONE',  ( 0.01496453197139708223, 5.000000000000000000, 5.196130874293197088 ) ) ;
#9970 = CARTESIAN_POINT ( 'NONE',  ( 3.749999999999999556, 9.249999999999998224, -3.500000000000000444 ) ) ;
#9971 = AXIS2_PLACEMENT_3D ( 'NONE', #10798, #6001, #14375 ) ;
#9972 = AXIS2_PLACEMENT_3D ( 'NONE', #8667, #13398, #11064 ) ;
#9973 = CARTESIAN_POINT ( 'NONE',  ( 12.41730312957572302, 2.668544226152360643, -166.2839238872912233 ) ) ;
#9974 = CARTESIAN_POINT ( 'NONE',  ( 7.534811383515542360, 0.1271246988106354836, -105.5137719823530205 ) ) ;
#9975 = CARTESIAN_POINT ( 'NONE',  ( -26.36649137993302361, 3.822280693179559147E-12, -175.2408862124428310 ) ) ;
#9976 = CARTESIAN_POINT ( 'NONE',  ( -1.376260179405573547, 0.000000000000000000, -106.6458321843530541 ) ) ;
#9977 = CARTESIAN_POINT ( 'NONE',  ( -30.85915506350906412, 15.00000000000000000, -156.4241655054801754 ) ) ;
#9978 = PRODUCT_RELATED_PRODUCT_CATEGORY ( 'detail', '', ( #5834 ) ) ;
#9979 = CARTESIAN_POINT ( 'NONE',  ( 3.749999999999999556, 12.25000000000000000, -3.500000000000000444 ) ) ;
#9980 = ORIENTED_EDGE ( 'NONE', *, *, #4492, .T. ) ;
#9981 = DIRECTION ( 'NONE',  ( 0.000000000000000000, 1.000000000000000000, 0.000000000000000000 ) ) ;
#9982 = CARTESIAN_POINT ( 'NONE',  ( 3.158384440324538467, -1.020558061026469288, -1.000000000000023537 ) ) ;
#9983 = CARTESIAN_POINT ( 'NONE',  ( -1.553300858899106629, 11.06250000000000000, 0.2500000000000002220 ) ) ;
#9984 = AXIS2_PLACEMENT_3D ( 'NONE', #11094, #5307, #514 ) ;
#9985 = CARTESIAN_POINT ( 'NONE',  ( -3.750000000000000000, 6.812500000000000000, -5.053300858899105741 ) ) ;
#9986 = CARTESIAN_POINT ( 'NONE',  ( -25.97807323962435078, 15.00000000000000000, -142.5647913107548277 ) ) ;
#9987 = CARTESIAN_POINT ( 'NONE',  ( -9.721966606022585111, 4.636404319106432581, -116.3614657654590587 ) ) ;
#9988 = CARTESIAN_POINT ( 'NONE',  ( 2.298097038856278029, 7.124999999999999112, -5.798097038856279362 ) ) ;
#9989 = EDGE_CURVE ( 'NONE', #2585, #9024, #6198, .T. ) ;
#9990 = CARTESIAN_POINT ( 'NONE',  ( -3.750000000000000000, 12.25000000000000000, -3.499999999999999112 ) ) ;
#9991 = CARTESIAN_POINT ( 'NONE',  ( -0.2500000000000000555, 4.500000000000000888, 1.500000000000000222 ) ) ;
#9992 = ADVANCED_FACE ( 'NONE', ( #6117 ), #332, .T. ) ;
#9993 = EDGE_CURVE ( 'NONE', #9140, #8581, #7741, .T. ) ;
#9994 = DIRECTION ( 'NONE',  ( 1.000000000000000000, 0.000000000000000000, 0.000000000000000000 ) ) ;
#9995 = APPROVAL_ROLE ( '' ) ;
#9996 = CARTESIAN_POINT ( 'NONE',  ( 3.249999999999999556, 11.75000000000000000, -3.500000000000000000 ) ) ;
#9997 = AXIS2_PLACEMENT_3D ( 'NONE', #7205, #15278, #5822 ) ;
#9998 = CARTESIAN_POINT ( 'NONE',  ( 7.352489943804302541, 2.075239479414269894, -39.38380306805896680 ) ) ;
#9999 = CARTESIAN_POINT ( 'NONE',  ( -20.05675593593863582, 15.00000000000000000, -128.8251628084967706 ) ) ;
#10000 = CARTESIAN_POINT ( 'NONE',  ( 10.27157762081180969, -3.902699979233760293E-12, -107.9972514637445329 ) ) ;
#10001 = PRODUCT_DEFINITION ( 'UNKNOWN', '', #10417, #10053 ) ;
#10002 = CARTESIAN_POINT ( 'NONE',  ( 26.15341798802279527, 6.000000000000000000, -138.7600702976168066 ) ) ;
#10003 = LINE ( 'NONE', #6597, #14323 ) ;
#10004 = ORIENTED_EDGE ( 'NONE', *, *, #10732, .F. ) ;
#10005 = CARTESIAN_POINT ( 'NONE',  ( 9.997152224788115049, 5.773884043947351330, -44.28753052795517675 ) ) ;
#10006 = ADVANCED_BREP_SHAPE_REPRESENTATION ( '', ( #12195, #9419 ), #11867 ) ;
#10007 = CARTESIAN_POINT ( 'NONE',  ( 4.917302814907795749, 15.00000000000000178, -102.2758535390863273 ) ) ;
#10008 = CARTESIAN_POINT ( 'NONE',  ( 2.651650429449552870, 11.12500000000000178, -6.151650429449553314 ) ) ;
#10009 = CARTESIAN_POINT ( 'NONE',  ( -2.298097038856278029, 11.62500000000000000, -1.201902961143720638 ) ) ;
#10010 = CARTESIAN_POINT ( 'NONE',  ( 2.298097038856278029, 13.12499999999999822, -5.798097038856279362 ) ) ;
#10011 = EDGE_LOOP ( 'NONE', ( #11625, #3239, #13344, #9541 ) ) ;
#10012 = CARTESIAN_POINT ( 'NONE',  ( -3.980102097228897245E-16, 9.500000000000000000, -6.749999999999999112 ) ) ;
#10013 = PLANE ( 'NONE',  #5209 ) ;
#10014 = EDGE_CURVE ( 'NONE', #6135, #13423, #9957, .T. ) ;
#10015 = CARTESIAN_POINT ( 'NONE',  ( -7.397649731168717935, 2.500000000000001332, -106.9840814774545237 ) ) ;
#10016 = CARTESIAN_POINT ( 'NONE',  ( -24.69661280395743574, 4.000000000000000888, -209.0572573213358396 ) ) ;
#10017 = APPROVAL ( #14203, 'UNSPECIFIED' ) ;
#10018 = CARTESIAN_POINT ( 'NONE',  ( 26.58801926426209405, 6.000000000000000000, -139.0072983920785532 ) ) ;
#10019 = ITEM_DEFINED_TRANSFORMATION ( 'NONE', 'NONE', #5969,  #9419 ) ;
#10020 = CARTESIAN_POINT ( 'NONE',  ( 8.930279828349792837, 15.00000000000000000, -123.5978143988205318 ) ) ;
#10021 = ORIENTED_EDGE ( 'NONE', *, *, #11469, .T. ) ;
#10022 = CARTESIAN_POINT ( 'NONE',  ( 3.249999999999999556, 5.750000000000000000, -3.500000000000000000 ) ) ;
#10023 = CARTESIAN_POINT ( 'NONE',  ( -1.553300858899106629, 13.06250000000000000, 0.2500000000000002220 ) ) ;
#10024 = ORIENTED_EDGE ( 'NONE', *, *, #8058, .F. ) ;
#10025 = DIRECTION ( 'NONE',  ( -0.02181900108494707127, 0.000000000000000000, 0.9997619372588930631 ) ) ;
#10026 = CARTESIAN_POINT ( 'NONE',  ( -2.651650429449553314, 0.3750000000000000555, -6.151650429449552426 ) ) ;
#10027 = CARTESIAN_POINT ( 'NONE',  ( -33.91109452335874153, 5.000000000000000888, -156.1716796081737471 ) ) ;
#10028 = CARTESIAN_POINT ( 'NONE',  ( 0.2402936566864277979, 0.3344966542995999603, 2.721810693018832161 ) ) ;
#10029 = CARTESIAN_POINT ( 'NONE',  ( -4.592425496802573972E-16, 0.5000000000000000000, -7.249999999999999112 ) ) ;
#10030 = DATE_AND_TIME ( #13816, #3031 ) ;
#10031 = CARTESIAN_POINT ( 'NONE',  ( 30.32986759126112730, 0.7500000000000000000, 46.54214087805580391 ) ) ;
#10032 = DIRECTION ( 'NONE',  ( -0.9510565162951488682, 0.000000000000000000, 0.3090169943749619952 ) ) ;
#10033 = ORIENTED_EDGE ( 'NONE', *, *, #1844, .T. ) ;
#10034 = CARTESIAN_POINT ( 'NONE',  ( 0.000000000000000000, 11.00000000000000000, -0.2500000000000002220 ) ) ;
#10035 = CARTESIAN_POINT ( 'NONE',  ( 0.000000000000000000, 0.2105996885190176970, -0.1347136637304948981 ) ) ;
#10036 = CARTESIAN_POINT ( 'NONE',  ( 1.346194077712558279, 5.062500000000000000, -6.750000000000000888 ) ) ;
#10037 = CARTESIAN_POINT ( 'NONE',  ( -1.346194077712558945, 11.56250000000000178, -0.2500000000000002220 ) ) ;
#10038 = CARTESIAN_POINT ( 'NONE',  ( -7.267596910945437472, 14.99999999999849187, -107.1579542029594876 ) ) ;
#10039 = DIRECTION ( 'NONE',  ( 0.003262051938530752433, 0.000000000000000000, 0.9999946794944213346 ) ) ;
#10040 = CARTESIAN_POINT ( 'NONE',  ( -3.249999999999999556, 5.187500000000001776, -2.153805922287440833 ) ) ;
#10041 = CARTESIAN_POINT ( 'NONE',  ( 3.749999999999999556, 4.249999999999999112, -3.500000000000000444 ) ) ;
#10042 = CARTESIAN_POINT ( 'NONE',  ( 0.000000000000000000, 8.000000000000000000, 0.2500000000000002220 ) ) ;
#10043 = VECTOR ( 'NONE', #163, 1000.000000000000000 ) ;
#10044 = DIRECTION ( 'NONE',  ( -0.000000000000000000, -0.000000000000000000, -1.000000000000000000 ) ) ;
#10045 = VERTEX_POINT ( 'NONE', #8588 ) ;
#10046 = CARTESIAN_POINT ( 'NONE',  ( 8.994679575448120801, -2.051692149507289097E-14, 14.93252568749840847 ) ) ;
#10047 = CARTESIAN_POINT ( 'NONE',  ( 2.651650429449552870, 9.125000000000000000, -6.151650429449555091 ) ) ;
#10048 = CARTESIAN_POINT ( 'NONE',  ( 3.659874141851102713, 14.82748211452489961, -0.4834174797602786011 ) ) ;
#10049 = DIRECTION ( 'NONE',  ( 0.000000000000000000, 0.000000000000000000, 1.000000000000000000 ) ) ;
#10050 = CARTESIAN_POINT ( 'NONE',  ( 10.55744226398496188, 2.749053926740207210, -106.8760807525077610 ) ) ;
#10051 = CARTESIAN_POINT ( 'NONE',  ( -9.605448531522425171, 8.673617379884035472E-16, -155.1394882739618311 ) ) ;
#10052 = CARTESIAN_POINT ( 'NONE',  ( 1.346194077712558279, 0.5625000000000002220, -6.750000000000000000 ) ) ;
#10053 = DESIGN_CONTEXT ( 'detailed design', #14617, 'design' ) ;
#10054 = VECTOR ( 'NONE', #6127, 1000.000000000000000 ) ;
#10055 = CARTESIAN_POINT ( 'NONE',  ( -42.91596092838683774, 9.999999999999998224, -158.7990843558010852 ) ) ;
#10056 = EDGE_CURVE ( 'NONE', #814, #9140, #3299, .T. ) ;
#10057 = CARTESIAN_POINT ( 'NONE',  ( 3.750000000000000000, 14.31250000000000355, -1.946699141100892705 ) ) ;
#10058 = ORIENTED_EDGE ( 'NONE', *, *, #13579, .T. ) ;
#10059 = CARTESIAN_POINT ( 'NONE',  ( 0.000000000000000000, 5.000000000000000888, -100.6237003951525679 ) ) ;
#10060 = CARTESIAN_POINT ( 'NONE',  ( 8.495120055765772449, 0.4951638288707319036, -105.5936704557864800 ) ) ;
#10061 = CARTESIAN_POINT ( 'NONE',  ( 3.749999999999999112, 10.31250000000000000, -1.946699141100893149 ) ) ;
#10062 =( REPRESENTATION_RELATIONSHIP ('NONE','NONE', #11394, #10891 ) REPRESENTATION_RELATIONSHIP_WITH_TRANSFORMATION ( #11919 )SHAPE_REPRESENTATION_RELATIONSHIP( ) );
#10063 = CARTESIAN_POINT ( 'NONE',  ( 26.73766085848597740, 5.000000000000000888, -138.7442440334353080 ) ) ;
#10064 = CARTESIAN_POINT ( 'NONE',  ( -3.980102097228897738E-16, 8.999999999999998224, -6.749999999999999112 ) ) ;
#10065 = DIRECTION ( 'NONE',  ( 0.000000000000000000, 0.8090169943749465631, 0.5877852522924742473 ) ) ;
#10066 = CARTESIAN_POINT ( 'NONE',  ( -1.553300858899106629, 14.06249999999999822, 0.2500000000000002220 ) ) ;
#10067 = CARTESIAN_POINT ( 'NONE',  ( -9.385448347264267355, 5.000000000000000888, -115.3551636530117150 ) ) ;
#10068 = APPROVAL ( #8478, 'UNSPECIFIED' ) ;
#10069 = CARTESIAN_POINT ( 'NONE',  ( 7.995229681650334541, 1.921202954650393924, -34.56909192082981974 ) ) ;
#10070 = CARTESIAN_POINT ( 'NONE',  ( -3.980102097228897245E-16, 12.50000000000000000, -6.749999999999999112 ) ) ;
#10071 = CARTESIAN_POINT ( 'NONE',  ( -0.3766621274091715987, 0.2694895414731200423, 0.07352276961066842031 ) ) ;
#10072 = FACE_OUTER_BOUND ( 'NONE', #3720, .T. ) ;
#10073 = CARTESIAN_POINT ( 'NONE',  ( 4.165694389856393620, 1.734723475976807094E-15, -108.8942237923054250 ) ) ;
#10074 = CARTESIAN_POINT ( 'NONE',  ( 2.011321487292375032, 5.000000000000000888, -137.8771695030452520 ) ) ;
#10075 = DIRECTION ( 'NONE',  ( -0.9961255586397056438, -0.000000000000000000, 0.08794243244722427244 ) ) ;
#10076 = ORIENTED_EDGE ( 'NONE', *, *, #6589, .T. ) ;
#10077 = ADVANCED_FACE ( 'NONE', ( #7188 ), #11911, .F. ) ;
#10078 = CARTESIAN_POINT ( 'NONE',  ( 8.990769910733003911, 12.49999999999999822, 0.3250886916252374026 ) ) ;
#10079 = CARTESIAN_POINT ( 'NONE',  ( 10.51703944396922275, 12.50000000000000000, -121.3897425166904469 ) ) ;
#10080 = CARTESIAN_POINT ( 'NONE',  ( 2.651650429449553759, 2.875000000000000000, -0.8483495705504471296 ) ) ;
#10081 = CARTESIAN_POINT ( 'NONE',  ( 2.298097038856278029, 10.12500000000000000, -5.798097038856279362 ) ) ;
#10082 = EDGE_CURVE ( 'NONE', #9716, #11175, #3727, .T. ) ;
#10083 = CARTESIAN_POINT ( 'NONE',  ( 1.346194077712560944, 0.9374999999999998890, -0.2500000000000010547 ) ) ;
#10084 = EDGE_LOOP ( 'NONE', ( #1635, #12476, #15001, #8148, #8433 ) ) ;
#10085 = CARTESIAN_POINT ( 'NONE',  ( 2.298097038856279362, 10.87500000000000178, -1.201902961143720860 ) ) ;
#10086 = CARTESIAN_POINT ( 'NONE',  ( 9.998602840258165259, 12.56502379761173671, -45.85452320410524862 ) ) ;
#10087 = CARTESIAN_POINT ( 'NONE',  ( -8.102584368418263239, 2.500000000000000888, -106.2168020716806467 ) ) ;
#10088 = LINE ( 'NONE', #11091, #4250 ) ;
#10089 = CARTESIAN_POINT ( 'NONE',  ( -8.611029641428904924, 12.67556477996888553, -115.7034661592606710 ) ) ;
#10090 = CONTEXT_DEPENDENT_SHAPE_REPRESENTATION ( #8972, #2382 ) ;
#10091 = CARTESIAN_POINT ( 'NONE',  ( 8.852045267489970115, 15.00000000000000178, -117.5747611283908043 ) ) ;
#10092 = CARTESIAN_POINT ( 'NONE',  ( 23.49624735387704533, 0.5263503646385538914, -138.0521088526025153 ) ) ;
#10093 = ORIENTED_EDGE ( 'NONE', *, *, #708, .T. ) ;
#10094 = CARTESIAN_POINT ( 'NONE',  ( 2.298097038856279362, 2.875000000000000000, -1.201902961143720860 ) ) ;
#10095 = CARTESIAN_POINT ( 'NONE',  ( -18.35446420518660560, 3.999999999999999112, -158.2547620175516272 ) ) ;
#10096 = CARTESIAN_POINT ( 'NONE',  ( -2.651650429449553314, 2.875000000000000000, -6.151650429449552426 ) ) ;
#10097 = EDGE_CURVE ( 'NONE', #10548, #2585, #13630, .T. ) ;
#10098 = ORIENTED_EDGE ( 'NONE', *, *, #8268, .F. ) ;
#10099 = LINE ( 'NONE', #12649, #13669 ) ;
#10100 = CARTESIAN_POINT ( 'NONE',  ( -2.651650429449553314, 3.375000000000000000, -6.151650429449552426 ) ) ;
#10101 = CARTESIAN_POINT ( 'NONE',  ( 26.13050938914192756, 4.000000000000000000, -138.2605953772281566 ) ) ;
#10102 = CARTESIAN_POINT ( 'NONE',  ( 2.757434015334491395, 0.1558106922034525610, 1.501509930864733056 ) ) ;
#10103 = CARTESIAN_POINT ( 'NONE',  ( -1.553300858899106407, 0.06250000000000002776, 0.2500000000000002220 ) ) ;
#10104 = APPLICATION_PROTOCOL_DEFINITION ( 'international standard', 'config_control_design', 1994, #4821 ) ;
#10105 = B_SPLINE_CURVE_WITH_KNOTS ( 'NONE', 3,
 ( #8205, #6754, #12937, #2117 ),
 .UNSPECIFIED., .F., .F.,
 ( 4, 4 ),
 ( 0.000000000000000000, 0.0005767408338914856592 ),
 .UNSPECIFIED. ) ;
#10106 = CARTESIAN_POINT ( 'NONE',  ( 11.65935602426492146, 5.000000000000001776, -123.2257483849739828 ) ) ;
#10107 = DIRECTION ( 'NONE',  ( 0.000000000000000000, 1.000000000000000000, 0.000000000000000000 ) ) ;
#10108 = VERTEX_POINT ( 'NONE', #7661 ) ;
#10109 = DIRECTION ( 'NONE',  ( 0.000000000000000000, 0.000000000000000000, 1.000000000000000000 ) ) ;
#10110 = CARTESIAN_POINT ( 'NONE',  ( 3.249999999999998224, 4.312500000000000000, -2.153805922287439945 ) ) ;
#10111 = CARTESIAN_POINT ( 'NONE',  ( 1.346194077712558279, 13.06249999999999822, -6.750000000000000888 ) ) ;
#10112 = CARTESIAN_POINT ( 'NONE',  ( 9.798257320807429949, 14.75244170371860797, -106.4031996619075073 ) ) ;
#10113 = CARTESIAN_POINT ( 'NONE',  ( 11.02703746864928469, 13.70076941827196393, -106.7007979685955661 ) ) ;
#10114 = CARTESIAN_POINT ( 'NONE',  ( -1.553300858899106629, 3.562500000000000888, 0.2499999999999998335 ) ) ;
#10115 = CARTESIAN_POINT ( 'NONE',  ( -3.750000000000000000, 8.187500000000000000, -1.946699141100892927 ) ) ;
#10116 = PRODUCT_DEFINITION_FORMATION_WITH_SPECIFIED_SOURCE ( 'ANY', '', #1532, .NOT_KNOWN. ) ;
#10117 = CARTESIAN_POINT ( 'NONE',  ( 10.99340860758277927, 5.943472311793079221, -45.60560901953395785 ) ) ;
#10118 = ORIENTED_EDGE ( 'NONE', *, *, #13703, .F. ) ;
#10119 = CARTESIAN_POINT ( 'NONE',  ( 1.990297875723435084, -2.051692149503915928E-14, 3.483276348926839461 ) ) ;
#10120 = CARTESIAN_POINT ( 'NONE',  ( 1.553300858899105963, 12.06250000000000000, -7.250000000000000888 ) ) ;
#10121 = CARTESIAN_POINT ( 'NONE',  ( 6.369258321017759350, -2.075239479414269894, -34.56909192082981974 ) ) ;
#10122 = CARTESIAN_POINT ( 'NONE',  ( 6.509216192753445540, 15.00000000000000178, -109.6918098674199911 ) ) ;
#10123 = CARTESIAN_POINT ( 'NONE',  ( 11.04730217088347466, 4.663186150664629714, -107.1178495010082514 ) ) ;
#10124 = VERTEX_POINT ( 'NONE', #3966 ) ;
#10125 = CARTESIAN_POINT ( 'NONE',  ( -13.29322798955594465, 4.000000000000054179, -151.9140868489417642 ) ) ;
#10126 = CARTESIAN_POINT ( 'NONE',  ( 1.052436484934206051, -2.075239479414269894, -1.000000000000021760 ) ) ;
#10127 = CC_DESIGN_APPROVAL ( #12916, ( #4938 ) ) ;
#10128 = CARTESIAN_POINT ( 'NONE',  ( 3.749999999999999112, 13.18750000000000000, -5.053300858899108405 ) ) ;
#10129 = ORIENTED_EDGE ( 'NONE', *, *, #11678, .T. ) ;
#10130 = DIRECTION ( 'NONE',  ( 8.764770998266003672E-18, -0.000000000000000000, 1.000000000000000000 ) ) ;
#10131 = FACE_OUTER_BOUND ( 'NONE', #14618, .T. ) ;
#10132 = AXIS2_PLACEMENT_3D ( 'NONE', #3972, #8677, #13412 ) ;
#10133 = CARTESIAN_POINT ( 'NONE',  ( -3.711466206438381654, 9.806991768140566279, -47.72538388426938383 ) ) ;
#10134 = CIRCLE ( 'NONE', #13107, 5.000000000000002665 ) ;
#10135 = B_SPLINE_CURVE_WITH_KNOTS ( 'NONE', 3,
 ( #4343, #561, #4191, #10060, #7580, #3167, #5272, #14796, #3029, #4269, #12374, #15018, #1791, #13629, #7736, #12456, #1873, #6578 ),
 .UNSPECIFIED., .F., .F.,
 ( 4, 2, 2, 2, 2, 2, 2, 2, 4 ),
 ( -1.729984944104041706E-05, 0.002003810841594060033, 0.003014366187111617960, 0.003519643859870403863, 0.004024921532629188899, 0.005035476878146755500, 0.006046032223664322101, 0.007056587569181887835, 0.008067142914699454437 ),
 .UNSPECIFIED. ) ;
#10136 = B_SPLINE_CURVE_WITH_KNOTS ( 'NONE', 3,
 ( #1092, #8190, #12917, #12840, #3331, #7094, #7172, #2331, #7029, #11893, #2175, #11742, #1235, #5943, #83, #4795, #3634, #1316 ),
 .UNSPECIFIED., .F., .F.,
 ( 4, 2, 2, 2, 2, 2, 2, 2, 4 ),
 ( 0.000000000000000000, 0.002451912426773313405, 0.004903824853546626811, 0.006129781066933302595, 0.007355737280319980115, 0.009807649707093331684, 0.01225956213386668325, 0.01471147456064003829, 0.01961529941418670847 ),
 .UNSPECIFIED. ) ;
#10137 = CYLINDRICAL_SURFACE ( 'NONE', #5513, 4.999999999999995559 ) ;
#10138 = CARTESIAN_POINT ( 'NONE',  ( 0.000000000000000000, 9.500000000000001776, -0.2500000000000002220 ) ) ;
#10139 = CARTESIAN_POINT ( 'NONE',  ( -4.492499072540820926, 5.000000000000000000, 2.611025101989610686 ) ) ;
#10140 = CARTESIAN_POINT ( 'NONE',  ( 3.750000000000000000, 13.75000000000000000, -3.500000000000000444 ) ) ;
#10141 = CARTESIAN_POINT ( 'NONE',  ( -68.82095148260327733, 9.999999999999998224, -201.5743162695746662 ) ) ;
#10142 = VECTOR ( 'NONE', #14426, 1000.000000000000000 ) ;
#10143 = CARTESIAN_POINT ( 'NONE',  ( -6.756410658677025616, 10.62990111995887865, -124.9665698180028670 ) ) ;
#10144 = EDGE_CURVE ( 'NONE', #5809, #7071, #9919, .T. ) ;
#10145 = VECTOR ( 'NONE', #11136, 1000.000000000000000 ) ;
#10146 = CARTESIAN_POINT ( 'NONE',  ( 3.249999999999998668, 11.68750000000000000, -4.846194077712560500 ) ) ;
#10147 = AXIS2_PLACEMENT_3D ( 'NONE', #718, #11227, #8981 ) ;
#10148 = CARTESIAN_POINT ( 'NONE',  ( -5.813579972774825855, 2.743867526398027223, -44.04909082593602676 ) ) ;
#10149 = PLANE ( 'NONE',  #2338 ) ;
#10150 = CARTESIAN_POINT ( 'NONE',  ( -1.346194077712559389, 8.062500000000000000, -0.2500000000000002220 ) ) ;
#10151 = CARTESIAN_POINT ( 'NONE',  ( -1.437999228988334544, 8.673617379884035472E-16, -140.6782968106692522 ) ) ;
#10152 = CARTESIAN_POINT ( 'NONE',  ( -7.751437813422534795, 10.00000000000000000, -124.5369783794910319 ) ) ;
#10153 = ORIENTED_EDGE ( 'NONE', *, *, #12794, .T. ) ;
#10154 = CARTESIAN_POINT ( 'NONE',  ( 8.963174318014939246, 12.17502284788009170, 1.589538110194233855 ) ) ;
#10155 = CARTESIAN_POINT ( 'NONE',  ( 1.171458888995337899, 15.00000000000000355, -111.2928373221764815 ) ) ;
#10156 = CARTESIAN_POINT ( 'NONE',  ( 3.749999999999999112, 1.812500000000000222, -1.946699141100892039 ) ) ;
#10157 = CARTESIAN_POINT ( 'NONE',  ( -3.750000000000000000, 1.812499999999999778, -5.053300858899105741 ) ) ;
#10158 = CARTESIAN_POINT ( 'NONE',  ( -3.249999999999999556, 1.187500000000000444, -2.153805922287440833 ) ) ;
#10159 = EDGE_LOOP ( 'NONE', ( #10232, #4506, #14536, #8258 ) ) ;
#10160 = AXIS2_PLACEMENT_3D ( 'NONE', #10221, #5643, #11295 ) ;
#10161 = CARTESIAN_POINT ( 'NONE',  ( -3.980102097228897245E-16, 10.50000000000000000, -6.749999999999999112 ) ) ;
#10162 = AXIS2_PLACEMENT_3D ( 'NONE', #11817, #4, #6810 ) ;
#10163 = CARTESIAN_POINT ( 'NONE',  ( 10.95283577138780728, 11.77391770468068088, -44.23857723416275434 ) ) ;
#10164 = CARTESIAN_POINT ( 'NONE',  ( -5.378945654756269512, 14.88217507582766963, -103.5310234877412796 ) ) ;
#10165 = EDGE_CURVE ( 'NONE', #12545, #10989, #12425, .T. ) ;
#10166 = CARTESIAN_POINT ( 'NONE',  ( 4.606088890118262391, 0.7456749647984134421, 2.303154267099985830 ) ) ;
#10167 = CARTESIAN_POINT ( 'NONE',  ( -9.385448346789152296, 10.36359568087253535, -115.3551636526205044 ) ) ;
#10168 = APPROVAL_DATE_TIME ( #14902, #15024 ) ;
#10169 = VECTOR ( 'NONE', #13743, 1000.000000000000000 ) ;
#10170 = B_SPLINE_CURVE_WITH_KNOTS ( 'NONE', 3,
 ( #6617, #11325, #11703, #4670, #10474, #9463, #1121, #5752 ),
 .UNSPECIFIED., .F., .F.,
 ( 4, 2, 2, 4 ),
 ( 0.002924603232979224900, 0.004377839289350649032, 0.005104457317536361532, 0.005831075345722074033 ),
 .UNSPECIFIED. ) ;
#10171 = CARTESIAN_POINT ( 'NONE',  ( 8.347943498143836294, 12.49999999999999822, -114.9028610997572457 ) ) ;
#10172 = CARTESIAN_POINT ( 'NONE',  ( -5.928758847211410554, 14.76754297112742798, -117.1828119328369553 ) ) ;
#10173 = ORIENTED_EDGE ( 'NONE', *, *, #5829, .T. ) ;
#10174 = CARTESIAN_POINT ( 'NONE',  ( 1.346194077712560944, 3.937500000000000000, -0.2500000000000010547 ) ) ;
#10175 = CARTESIAN_POINT ( 'NONE',  ( -30.40484592373450212, 4.000000000000000888, -187.9928767041745061 ) ) ;
#10176 = CARTESIAN_POINT ( 'NONE',  ( 3.749999999999999112, 1.187500000000000222, -5.053300858899108405 ) ) ;
#10177 = ORIENTED_EDGE ( 'NONE', *, *, #4765, .T. ) ;
#10178 = CARTESIAN_POINT ( 'NONE',  ( 0.000000000000000000, 5.000000000000000000, 0.000000000000000000 ) ) ;
#10179 = APPROVAL ( #14676, 'UNSPECIFIED' ) ;
#10180 = SECURITY_CLASSIFICATION ( '', '', #13990 ) ;
#10181 = CARTESIAN_POINT ( 'NONE',  ( 2.651650429449552870, 4.625000000000000000, -6.151650429449554203 ) ) ;
#10182 = FACE_OUTER_BOUND ( 'NONE', #10613, .T. ) ;
#10183 = EDGE_CURVE ( 'NONE', #8015, #2663, #1076, .T. ) ;
#10184 = CARTESIAN_POINT ( 'NONE',  ( 2.530298019944475563, 8.673617379884035472E-16, 0.2330448234422082265 ) ) ;
#10185 = CARTESIAN_POINT ( 'NONE',  ( 11.14636119983888385, 3.654497975985243841, -106.3565569454754041 ) ) ;
#10186 = ADVANCED_FACE ( 'NONE', ( #7511 ), #12229, .T. ) ;
#10187 = PERSON_AND_ORGANIZATION_ROLE ( 'design_supplier' ) ;
#10188 = ADVANCED_FACE ( 'NONE', ( #641 ), #3394, .F. ) ;
#10189 = CARTESIAN_POINT ( 'NONE',  ( 8.563244450085640835, 5.000000000000000000, -111.6252051639990981 ) ) ;
#10190 = DIRECTION ( 'NONE',  ( -0.000000000000000000, 1.000000000000000000, -0.000000000000000000 ) ) ;
#10191 = ORIENTED_EDGE ( 'NONE', *, *, #708, .F. ) ;
#10192 = DIRECTION ( 'NONE',  ( 0.7859448108640930686, 0.000000000000000000, -0.6182966555592913638 ) ) ;
#10193 = CARTESIAN_POINT ( 'NONE',  ( -2.298097038856279362, 4.875000000000000000, -5.798097038856278473 ) ) ;
#10194 = CARTESIAN_POINT ( 'NONE',  ( 4.516549078349731516, 2.547190344450775967, -1.663700395152574396 ) ) ;
#10195 = AXIS2_PLACEMENT_3D ( 'NONE', #8708, #2849, #7548 ) ;
#10196 = CARTESIAN_POINT ( 'NONE',  ( -7.754603562235517167, 2.500000000000000444, -121.4663199874671307 ) ) ;
#10197 = CARTESIAN_POINT ( 'NONE',  ( 3.749999999999999112, 4.312500000000000000, -1.946699141100893149 ) ) ;
#10198 = CARTESIAN_POINT ( 'NONE',  ( 2.651650429449552870, 11.62500000000000000, -6.151650429449554203 ) ) ;
#10199 = CARTESIAN_POINT ( 'NONE',  ( -3.214905123735726900, 2.559042896907052889, -1.000000000000011768 ) ) ;
#10200 = ORIENTED_EDGE ( 'NONE', *, *, #8092, .T. ) ;
#10201 = CARTESIAN_POINT ( 'NONE',  ( -3.813985985191490347, 9.650666666666664284, -43.20108978589184545 ) ) ;
#10202 = CARTESIAN_POINT ( 'NONE',  ( -1.553300858899107073, 10.93750000000000000, -7.249999999999999112 ) ) ;
#10203 = LINE ( 'NONE', #701, #1581 ) ;
#10204 = CARTESIAN_POINT ( 'NONE',  ( 6.843830495165342143, 15.00000000000000000, -108.8700626460535261 ) ) ;
#10205 = CIRCLE ( 'NONE', #5029, 3.500000000000013323 ) ;
#10206 = DIRECTION ( 'NONE',  ( -0.000000000000000000, -1.000000000000000000, -0.000000000000000000 ) ) ;
#10207 = VERTEX_POINT ( 'NONE', #1794 ) ;
#10208 = CARTESIAN_POINT ( 'NONE',  ( -23.09901293210274886, 3.999999999999755307, -165.9319877299972461 ) ) ;
#10209 = DIRECTION ( 'NONE',  ( 0.000000000000000000, 1.000000000000000000, 0.000000000000000000 ) ) ;
#10210 = CARTESIAN_POINT ( 'NONE',  ( -39.01706460775102414, 15.00000000000000000, -156.9624841731871072 ) ) ;
#10211 = CARTESIAN_POINT ( 'NONE',  ( 3.249999999999999556, 4.250000000000000000, -3.500000000000000000 ) ) ;
#10212 = ORIENTED_EDGE ( 'NONE', *, *, #6310, .T. ) ;
#10213 = CARTESIAN_POINT ( 'NONE',  ( -9.110371329404767238, 15.00000000000119194, -123.5182978442195463 ) ) ;
#10214 = DIRECTION ( 'NONE',  ( 0.000000000000000000, -1.000000000000000000, 0.000000000000000000 ) ) ;
#10215 = CARTESIAN_POINT ( 'NONE',  ( -25.68413237157757933, 0.4228586813406581824, -203.6825093939540920 ) ) ;
#10216 = CARTESIAN_POINT ( 'NONE',  ( -1.346194077712559389, 10.43750000000000000, -6.749999999999999112 ) ) ;
#10217 = CARTESIAN_POINT ( 'NONE',  ( 6.122889832264990062, 9.999999999999761968, 5.281130614573721793 ) ) ;
#10218 = AXIS2_PLACEMENT_3D ( 'NONE', #6355, #7583, #6427 ) ;
#10219 = CARTESIAN_POINT ( 'NONE',  ( 1.346194077712558279, 10.06250000000000000, -6.750000000000000888 ) ) ;
#10220 = CIRCLE ( 'NONE', #11448, 5.000000000000000888 ) ;
#10221 = CARTESIAN_POINT ( 'NONE',  ( 51.19063959271458231, 0.000000000000000000, 70.12932606827693860 ) ) ;
#10222 = CARTESIAN_POINT ( 'NONE',  ( 0.000000000000000000, -0.4999999999999999445, 0.2500000000000002220 ) ) ;
#10223 = DIRECTION ( 'NONE',  ( 1.000000000000000000, 0.000000000000000000, 0.000000000000000000 ) ) ;
#10224 = CARTESIAN_POINT ( 'NONE',  ( -5.622987266627582414, 14.75541105728024682, -103.8730693452872771 ) ) ;
#10225 = CARTESIAN_POINT ( 'NONE',  ( 2.298097038856279362, 13.87500000000000000, -1.201902961143720860 ) ) ;
#10226 = DIRECTION ( 'NONE',  ( -0.000000000000000000, 1.000000000000000000, -0.000000000000000000 ) ) ;
#10227 = CARTESIAN_POINT ( 'NONE',  ( 1.500000000000000000, 4.500000000000000888, 0.2500000000000002220 ) ) ;
#10228 = CARTESIAN_POINT ( 'NONE',  ( -2.298097038856278918, 10.37500000000000000, -5.798097038856277585 ) ) ;
#10229 = CIRCLE ( 'NONE', #6761, 14.80000000000025651 ) ;
#10230 = CARTESIAN_POINT ( 'NONE',  ( 27.03835354040193195, 5.000000000000000888, -138.2189567750509980 ) ) ;
#10231 = CARTESIAN_POINT ( 'NONE',  ( 8.881449363785039353, 15.00000000000000000, -2.080517014814270205 ) ) ;
#10232 = ORIENTED_EDGE ( 'NONE', *, *, #13499, .T. ) ;
#10233 = CARTESIAN_POINT ( 'NONE',  ( -5.309262520577839872, 6.000000000000000000, -125.0911079416483176 ) ) ;
#10234 = CARTESIAN_POINT ( 'NONE',  ( 3.391286578035700217, 15.00000000000000000, -107.3770126362747419 ) ) ;
#10235 = CARTESIAN_POINT ( 'NONE',  ( -2.651650429449552870, 14.62500000000000178, -0.8483495705504467965 ) ) ;
#10236 = CARTESIAN_POINT ( 'NONE',  ( 3.249999999999999556, 14.25000000000000178, -3.500000000000000000 ) ) ;
#10237 = CARTESIAN_POINT ( 'NONE',  ( -3.249999999999999112, 13.68750000000000178, -2.153805922287440833 ) ) ;
#10238 = EDGE_LOOP ( 'NONE', ( #7873, #8328, #14888, #4215 ) ) ;
#10239 = CARTESIAN_POINT ( 'NONE',  ( 3.249999999999999556, 12.75000000000000178, -3.500000000000000000 ) ) ;
#10240 = VECTOR ( 'NONE', #11942, 999.9999999999998863 ) ;
#10241 = CARTESIAN_POINT ( 'NONE',  ( 10.00293577155236235, 11.69603995595522505, -43.86820082419217925 ) ) ;
#10242 = CARTESIAN_POINT ( 'NONE',  ( -8.373832254232995709, 12.83239838503939900, -104.7981674252878008 ) ) ;
#10243 = CARTESIAN_POINT ( 'NONE',  ( -6.679542461294499134, 14.42304080565615543, -116.5285319886262414 ) ) ;
#10244 = DATE_AND_TIME ( #13580, #11346 ) ;
#10245 = CARTESIAN_POINT ( 'NONE',  ( 9.146012981092644267, 12.49999999999999822, -118.4481327388941025 ) ) ;
#10246 = DIRECTION ( 'NONE',  ( 0.000000000000000000, 0.000000000000000000, 1.000000000000000000 ) ) ;
#10247 = CARTESIAN_POINT ( 'NONE',  ( 25.70480266353256482, 2.194422113504707283, -137.2509578016119463 ) ) ;
#10248 = ORIENTED_EDGE ( 'NONE', *, *, #6779, .F. ) ;
#10249 = CARTESIAN_POINT ( 'NONE',  ( -3.980102097228897245E-16, 3.500000000000000000, -6.749999999999999112 ) ) ;
#10250 = DIRECTION ( 'NONE',  ( 0.000000000000000000, -1.000000000000000000, 0.000000000000000000 ) ) ;
#10251 = CARTESIAN_POINT ( 'NONE',  ( -2.651650429449552870, 2.625000000000000000, -0.8483495705504463524 ) ) ;
#10252 = VERTEX_POINT ( 'NONE', #1640 ) ;
#10253 = EDGE_CURVE ( 'NONE', #15113, #13758, #13677, .T. ) ;
#10254 = CARTESIAN_POINT ( 'NONE',  ( -5.525175898872149105, 14.85443352937157790, -116.9935625178452057 ) ) ;
#10255 = DIRECTION ( 'NONE',  ( 0.02181900108494707474, 0.000000000000000000, -0.9997619372588932851 ) ) ;
#10256 = CARTESIAN_POINT ( 'NONE',  ( -2.651650429449553314, 6.375000000000000888, -6.151650429449552426 ) ) ;
#10257 = CARTESIAN_POINT ( 'NONE',  ( -25.68068971291294744, 0.4053893758593278274, -203.6019930943793383 ) ) ;
#10258 = CARTESIAN_POINT ( 'NONE',  ( 0.2611509734078907852, 4.672652403575303204, 2.958061905235128464 ) ) ;
#10259 = DATE_AND_TIME ( #11262, #12835 ) ;
#10260 = CARTESIAN_POINT ( 'NONE',  ( 19.68155780323316151, 5.000000000000001776, -131.7762816226957057 ) ) ;
#10261 = ORIENTED_EDGE ( 'NONE', *, *, #14749, .F. ) ;
#10262 = CARTESIAN_POINT ( 'NONE',  ( -1.346194077712558945, 4.562500000000000000, -0.2500000000000002220 ) ) ;
#10263 = ADVANCED_FACE ( 'NONE', ( #1874 ), #6579, .F. ) ;
#10264 = EDGE_CURVE ( 'NONE', #114, #1674, #12945, .T. ) ;
#10265 = CARTESIAN_POINT ( 'NONE',  ( 1.553300858899105963, 11.06250000000000178, -7.249999999999999112 ) ) ;
#10266 = CARTESIAN_POINT ( 'NONE',  ( 2.651650429449552870, 13.62500000000000000, -6.151650429449554203 ) ) ;
#10267 = LINE ( 'NONE', #11203, #13612 ) ;
#10268 = ORIENTED_EDGE ( 'NONE', *, *, #161, .T. ) ;
#10269 = CARTESIAN_POINT ( 'NONE',  ( 29.71057115341583454, -2.051692149507289097E-14, 36.39324188472026123 ) ) ;
#10270 = CARTESIAN_POINT ( 'NONE',  ( -3.249999999999999112, 0.8125000000000001110, -4.846194077712558723 ) ) ;
#10271 = CARTESIAN_POINT ( 'NONE',  ( 26.04203104729492679, 0.000000000000000000, 69.41411580402544246 ) ) ;
#10272 = PERSON_AND_ORGANIZATION ( #3176, #3020 ) ;
#10273 = DIRECTION ( 'NONE',  ( 0.000000000000000000, 1.000000000000000000, 0.000000000000000000 ) ) ;
#10274 = DIRECTION ( 'NONE',  ( 0.9989498407774403121, 0.000000000000000000, 0.04581719776161458091 ) ) ;
#10275 = ORIENTED_EDGE ( 'NONE', *, *, #2622, .T. ) ;
#10276 = CARTESIAN_POINT ( 'NONE',  ( -26.45842032310348202, 3.999999999998672617, -207.8493744993166672 ) ) ;
#10277 = CARTESIAN_POINT ( 'NONE',  ( 12.50482138048521641, 2.904909039721687236, -166.3652064813286700 ) ) ;
#10278 = CARTESIAN_POINT ( 'NONE',  ( -33.77251566124358817, 9.999999999999998224, -156.1614337057717989 ) ) ;
#10279 = CARTESIAN_POINT ( 'NONE',  ( -1.346194077712558945, 4.562500000000000000, -0.2500000000000002220 ) ) ;
#10280 = EDGE_LOOP ( 'NONE', ( #5064, #15016, #10965, #12318 ) ) ;
#10281 = CARTESIAN_POINT ( 'NONE',  ( 0.000000000000000000, 1.530808498934191509E-17, 0.000000000000000000 ) ) ;
#10282 = CARTESIAN_POINT ( 'NONE',  ( 1.893911505664648054, 9.999999999999998224, -1.663006917529762152 ) ) ;
#10283 = ADVANCED_FACE ( 'NONE', ( #14874 ), #791, .T. ) ;
#10284 = CARTESIAN_POINT ( 'NONE',  ( 1.320501113854931408, 15.00000000000000000, -137.8664870916819893 ) ) ;
#10285 = CARTESIAN_POINT ( 'NONE',  ( 6.122889832127041743, 10.32785525203418509, 5.281130614556315273 ) ) ;
#10286 = CARTESIAN_POINT ( 'NONE',  ( -6.310237929021329961, 1.734723475976807094E-15, -119.2996315833885035 ) ) ;
#10287 = CARTESIAN_POINT ( 'NONE',  ( -3.249999999999999112, 12.68750000000000178, -2.153805922287440833 ) ) ;
#10288 = LINE ( 'NONE', #3107, #8166 ) ;
#10289 = CARTESIAN_POINT ( 'NONE',  ( -1.553300858899106629, 12.06250000000000000, 0.2500000000000002220 ) ) ;
#10290 = FACE_OUTER_BOUND ( 'NONE', #1486, .T. ) ;
#10291 = DIRECTION ( 'NONE',  ( 0.000000000000000000, 0.000000000000000000, -1.000000000000000000 ) ) ;
#10292 = DIRECTION ( 'NONE',  ( -1.000000000000000000, 0.000000000000000000, 0.000000000000000000 ) ) ;
#10293 = CARTESIAN_POINT ( 'NONE',  ( -8.918093633295288925, 10.00000000000000355, -123.2478653285129724 ) ) ;
#10294 = CARTESIAN_POINT ( 'NONE',  ( 8.895558325401111688, 6.000000000000000000, -125.4560052468458906 ) ) ;
#10295 = CARTESIAN_POINT ( 'NONE',  ( 1.346194077712560944, 6.937500000000000000, -0.2500000000000010547 ) ) ;
#10296 = CARTESIAN_POINT ( 'NONE',  ( 2.543998210650478597, 8.673617379884035472E-16, -136.5336064733026831 ) ) ;
#10297 = ORIENTED_EDGE ( 'NONE', *, *, #4344, .F. ) ;
#10298 = EDGE_LOOP ( 'NONE', ( #13665, #14492, #11178, #15227 ) ) ;
#10299 = CARTESIAN_POINT ( 'NONE',  ( -3.025102703132700022, 15.00000000000000000, -116.3639557890653577 ) ) ;
#10300 = CARTESIAN_POINT ( 'NONE',  ( 0.000000000000000000, 3.000000000000000000, 0.2500000000000002220 ) ) ;
#10301 = CARTESIAN_POINT ( 'NONE',  ( 2.298097038856278029, 14.12500000000000000, -5.798097038856279362 ) ) ;
#10302 = CARTESIAN_POINT ( 'NONE',  ( -1.376260179405573547, 0.000000000000000000, -106.6458321843530541 ) ) ;
#10303 = ORIENTED_EDGE ( 'NONE', *, *, #11927, .F. ) ;
#10304 =( BOUNDED_SURFACE ( )  B_SPLINE_SURFACE ( 3, 2, ( 
 ( #3547, #9421, #3468 ),
 ( #12905, #3320, #8030 ),
 ( #8254, #12755, #2318 ),
 ( #10429, #15166, #11803 ),
 ( #1219, #15010, #4561 ),
 ( #4403, #11731, #9270 ),
 ( #13994, #8102, #2618 ),
 ( #14379, #12199, #14537 ),
 ( #11881, #1455, #10655 ),
 ( #8557, #302, #7159 ),
 ( #6249, #13133, #8485 ),
 ( #144, #7321, #14291 ),
 ( #4930, #13050, #5929 ),
 ( #384, #8401, #4854 ),
 ( #9495, #3777, #13216 ),
 ( #5015, #7245, #14220 ),
 ( #6162, #12118, #12034 ),
 ( #10730, #3934, #10882 ),
 ( #9647, #69, #8636 ),
 ( #9734, #3692, #2543 ),
 ( #2462, #4781, #14463 ),
 ( #11958, #2777, #1382 ),
 ( #1303, #6084, #10801 ),
 ( #9565, #3859, #215 ),
 ( #1535, #13292, #7481 ),
 ( #13372, #2696, #3621 ),
 ( #8324, #7395, #10966 ),
 ( #6006, #5093, #9806 ) ),
 .UNSPECIFIED., .F., .F., .T. ) 
 B_SPLINE_SURFACE_WITH_KNOTS ( ( 4, 2, 2, 2, 2, 2, 2, 2, 2, 2, 2, 2, 2, 4 ),
 ( 3, 3 ),
 ( 0.000000000000000000, 0.0003820775045722776039, 0.0007641550091445552077, 0.001146232513716832812, 0.001337271266002971505, 0.001528310018289110415, 0.001910387522861388019, 0.002292465027433665623, 0.003056620036578220831, 0.003438697541150498652, 0.003820775045722776039, 0.004584930054867331246, 0.005349085064011886020, 0.006113240073156441662 ),
 ( 0.000000000000000000, 1.000000000000000000 ),
 .UNSPECIFIED. ) 
 GEOMETRIC_REPRESENTATION_ITEM ( )  RATIONAL_B_SPLINE_SURFACE ( (
 ( 1.000000000000000000, 0.6694682279269816849, 1.000000000000000000),
 ( 1.000000000000000000, 0.6694688976805022174, 1.000000000000000000),
 ( 1.000000000000000000, 0.6718652449342649158, 1.000000000000000000),
 ( 1.000000000000000000, 0.6808533733821083844, 1.000000000000000000),
 ( 1.000000000000000000, 0.6875604826314558604, 1.000000000000000000),
 ( 1.000000000000000000, 0.7038992507919969999, 1.000000000000000000),
 ( 1.000000000000000000, 0.7134862437630616894, 1.000000000000000000),
 ( 1.000000000000000000, 0.7292503528835072579, 1.000000000000000000),
 ( 1.000000000000000000, 0.7347607280474764968, 1.000000000000000000),
 ( 1.000000000000000000, 0.7459493779136278091, 1.000000000000000000),
 ( 1.000000000000000000, 0.7516437210088404708, 1.000000000000000000),
 ( 1.000000000000000000, 0.7688860810062153606, 1.000000000000000000),
 ( 1.000000000000000000, 0.7805878518874648231, 1.000000000000000000),
 ( 1.000000000000000000, 0.8038470659974755739, 1.000000000000000000),
 ( 1.000000000000000000, 0.8154457322603761993, 1.000000000000000000),
 ( 1.000000000000000000, 0.8485885531796709680, 1.000000000000000000),
 ( 1.000000000000000000, 0.8687647592111614747, 1.000000000000000000),
 ( 1.000000000000000000, 0.8953432496372137894, 1.000000000000000000),
 ( 1.000000000000000000, 0.9036225306460309303, 1.000000000000000000),
 ( 1.000000000000000000, 0.9186755269451735151, 1.000000000000000000),
 ( 1.000000000000000000, 0.9254787334919890585, 1.000000000000000000),
 ( 1.000000000000000000, 0.9438496984080199104, 1.000000000000000000),
 ( 1.000000000000000000, 0.9533694582932917827, 1.000000000000000000),
 ( 1.000000000000000000, 0.9678894448523732708, 1.000000000000000000),
 ( 1.000000000000000000, 0.9728964749375748067, 1.000000000000000000),
 ( 1.000000000000000000, 0.9793693877884432908, 1.000000000000000000),
 ( 1.000000000000000000, 0.9809066217507083074, 1.000000000000000000),
 ( 1.000000000000000000, 0.9811261306835751261, 1.000000000000000000) ) ) 
 REPRESENTATION_ITEM ( '' )  SURFACE ( )  );
#10305 = CARTESIAN_POINT ( 'NONE',  ( -3.249999999999999556, 9.312499999999998224, -4.846194077712557835 ) ) ;
#10306 = CARTESIAN_POINT ( 'NONE',  ( 8.881449363785039353, 5.000000000000000888, -2.080517014814270205 ) ) ;
#10307 = CARTESIAN_POINT ( 'NONE',  ( -8.851953732384830076, 10.69856349026787612, -105.4975849175705918 ) ) ;
#10308 = CARTESIAN_POINT ( 'NONE',  ( -3.520407287333055635, 7.379999999999995453, -45.56125597433126018 ) ) ;
#10309 = PERSON_AND_ORGANIZATION_ROLE ( 'classification_officer' ) ;
#10310 = CARTESIAN_POINT ( 'NONE',  ( 6.453443679602843375, 15.00000000000000000, -109.8021161339212455 ) ) ;
#10311 = CARTESIAN_POINT ( 'NONE',  ( 6.369258321017759350, 2.075239479414269894, -34.56909192082981974 ) ) ;
#10312 = ORIENTED_EDGE ( 'NONE', *, *, #5175, .F. ) ;
#10313 = CARTESIAN_POINT ( 'NONE',  ( 24.10521022763708743, 0.8297099929889686365, -137.8334368346246492 ) ) ;
#10314 = CARTESIAN_POINT ( 'NONE',  ( -1.346194077712558945, 11.06250000000000000, -0.2500000000000002220 ) ) ;
#10315 = ORIENTED_EDGE ( 'NONE', *, *, #12923, .F. ) ;
#10316 = VERTEX_POINT ( 'NONE', #11145 ) ;
#10317 = CARTESIAN_POINT ( 'NONE',  ( -3.249999999999999556, 4.250000000000000000, -3.499999999999999556 ) ) ;
#10318 = DIRECTION ( 'NONE',  ( 0.000000000000000000, 0.000000000000000000, 1.000000000000000000 ) ) ;
#10319 = CARTESIAN_POINT ( 'NONE',  ( -1.553300858899106629, 2.562500000000000444, 0.2500000000000002220 ) ) ;
#10320 = CARTESIAN_POINT ( 'NONE',  ( 1.346194077712558279, 6.062500000000000888, -6.750000000000000888 ) ) ;
#10321 = ORIENTED_EDGE ( 'NONE', *, *, #1112, .F. ) ;
#10322 = DIRECTION ( 'NONE',  ( -1.000000000000000000, 0.000000000000000000, 0.000000000000000000 ) ) ;
#10323 = DIRECTION ( 'NONE',  ( 0.000000000000000000, 0.000000000000000000, -1.000000000000000000 ) ) ;
#10324 = CARTESIAN_POINT ( 'NONE',  ( 2.651650429449553759, 4.875000000000000000, -0.8483495705504471296 ) ) ;
#10325 = CARTESIAN_POINT ( 'NONE',  ( -25.22140796077621872, 1.064333479732355909E-15, -199.9032618446891547 ) ) ;
#10326 = CARTESIAN_POINT ( 'NONE',  ( -0.2500000000000000555, 4.500000000000000888, 0.2500000000000002220 ) ) ;
#10327 = DATE_AND_TIME ( #6923, #13587 ) ;
#10328 = ADVANCED_FACE ( 'NONE', ( #9349 ), #1158, .F. ) ;
#10329 = CARTESIAN_POINT ( 'NONE',  ( -3.854019100140201104, 2.352429041693352652, -1.000000000000004441 ) ) ;
#10330 = CARTESIAN_POINT ( 'NONE',  ( 28.21756277010331004, 6.321094445766561876, -25.21174485404201704 ) ) ;
#10331 = ORIENTED_EDGE ( 'NONE', *, *, #1963, .T. ) ;
#10332 = CARTESIAN_POINT ( 'NONE',  ( 2.298097038856279362, 6.374999999999999112, -1.201902961143720860 ) ) ;
#10333 = DIRECTION ( 'NONE',  ( 0.02181900108494707127, 0.000000000000000000, -0.9997619372588931741 ) ) ;
#10334 = CARTESIAN_POINT ( 'NONE',  ( -3.749999999999999556, 9.750000000000000000, -3.499999999999999112 ) ) ;
#10335 = CARTESIAN_POINT ( 'NONE',  ( -65.20864362898224442, 14.64660082145764619, -194.2756847103777318 ) ) ;
#10336 = ORIENTED_EDGE ( 'NONE', *, *, #4932, .F. ) ;
#10337 = CARTESIAN_POINT ( 'NONE',  ( 0.7644969749116201641, 4.641615622421193521, -138.4027240657578375 ) ) ;
#10338 = CARTESIAN_POINT ( 'NONE',  ( -1.553300858899106629, 12.56250000000000355, 0.2500000000000002220 ) ) ;
#10339 = CARTESIAN_POINT ( 'NONE',  ( -3.376139687035127235, 4.336808689942017736E-16, -108.9613800447800003 ) ) ;
#10340 = APPLICATION_CONTEXT ( 'configuration controlled 3d designs of mechanical parts and assemblies' ) ;
#10341 = PERSON_AND_ORGANIZATION ( #3176, #3020 ) ;
#10342 = EDGE_CURVE ( 'NONE', #6678, #8603, #8108, .T. ) ;
#10343 = PLANE ( 'NONE',  #7648 ) ;
#10344 = B_SPLINE_CURVE_WITH_KNOTS ( 'NONE', 3,
 ( #775, #1858, #5402, #6409, #13687, #10117 ),
 .UNSPECIFIED., .F., .F.,
 ( 4, 2, 4 ),
 ( 0.000000000000000000, 0.001008764465307790880, 0.002017528930615581761 ),
 .UNSPECIFIED. ) ;
#10345 = B_SPLINE_CURVE_WITH_KNOTS ( 'NONE', 3,
 ( #7224, #2214, #202, #10633, #8237, #12810, #3677, #11645, #12890, #127, #11718, #7070, #53, #2372, #4914, #3375 ),
 .UNSPECIFIED., .F., .F.,
 ( 4, 2, 2, 2, 2, 2, 2, 4 ),
 ( 0.000000000000000000, 0.005034478876242980301, 0.01006895775248596060, 0.02013791550497199406, 0.02517239438121500819, 0.03020687325745802579, 0.03524135213370103992, 0.04027583100994405751 ),
 .UNSPECIFIED. ) ;
#10346 = VERTEX_POINT ( 'NONE', #5639 ) ;
#10347 = CARTESIAN_POINT ( 'NONE',  ( -27.36259546841008827, 1.380486956869476911E-13, -204.7781919227250853 ) ) ;
#10348 = DIRECTION ( 'NONE',  ( 0.000000000000000000, 0.000000000000000000, -1.000000000000000000 ) ) ;
#10349 = CARTESIAN_POINT ( 'NONE',  ( -64.40997231175244053, 15.00000000000000000, -182.5864378953727396 ) ) ;
#10350 = CARTESIAN_POINT ( 'NONE',  ( -2.298097038856279362, 1.874999999999999778, -5.798097038856278473 ) ) ;
#10351 = ORIENTED_EDGE ( 'NONE', *, *, #13747, .F. ) ;
#10352 = CARTESIAN_POINT ( 'NONE',  ( -5.080258480092867401, 15.00000000000000000, -126.4829214896701899 ) ) ;
#10353 = CARTESIAN_POINT ( 'NONE',  ( -10.50399746317070715, 15.00000000000000178, -142.5005062768583741 ) ) ;
#10354 = CARTESIAN_POINT ( 'NONE',  ( 1.346194077712558057, 10.56250000000000000, -6.750000000000000000 ) ) ;
#10355 = CC_DESIGN_APPROVAL ( #11573, ( #8377 ) ) ;
#10356 = CARTESIAN_POINT ( 'NONE',  ( 8.976478810040582346, 15.03641560954238088, 0.9799169515470964598 ) ) ;
#10357 = CARTESIAN_POINT ( 'NONE',  ( -2.027137927904086201, 5.000000000000000888, -107.0032022124503044 ) ) ;
#10358 = CARTESIAN_POINT ( 'NONE',  ( 2.298097038856278029, 12.12500000000000000, -5.798097038856279362 ) ) ;
#10359 = TOROIDAL_SURFACE ( 'NONE', #5903, 2.250000000000003553, 1.000000000000000000 ) ;
#10360 = CC_DESIGN_DATE_AND_TIME_ASSIGNMENT ( #3659, #7361, ( #7654 ) ) ;
#10361 = CARTESIAN_POINT ( 'NONE',  ( 6.089666224640344794, 0.000000000000000000, -124.6062682140657074 ) ) ;
#10362 = CARTESIAN_POINT ( 'NONE',  ( 0.000000000000000000, 1.500000000000000222, 0.2500000000000002220 ) ) ;
#10363 = CARTESIAN_POINT ( 'NONE',  ( 0.2625675443133231868, 10.25843542206809822, 2.974107430077547409 ) ) ;
#10364 = CARTESIAN_POINT ( 'NONE',  ( -6.790153584124030139, 10.31788924015992137, -124.9643354754709748 ) ) ;
#10365 = ADVANCED_FACE ( 'NONE', ( #9276 ), #5523, .T. ) ;
#10366 = EDGE_CURVE ( 'NONE', #40, #2594, #133, .T. ) ;
#10367 = DIRECTION ( 'NONE',  ( 0.000000000000000000, 0.000000000000000000, 1.000000000000000000 ) ) ;
#10368 = EDGE_CURVE ( 'NONE', #13477, #4330, #5568, .T. ) ;
#10369 = ORGANIZATION ( 'NAUO-ORG8', 'UNSPECIFIED', 'UNSPECIFIED' ) ;
#10370 = CARTESIAN_POINT ( 'NONE',  ( 13.59058908281841482, 2.099999999999187850, 61.49439185523788609 ) ) ;
#10371 = CARTESIAN_POINT ( 'NONE',  ( -3.249999999999999556, 7.250000000000000000, -3.499999999999999556 ) ) ;
#10372 = CIRCLE ( 'NONE', #259, 2.000000000000000000 ) ;
#10373 = CARTESIAN_POINT ( 'NONE',  ( 26.88776758612647200, 5.000000000000000888, -138.4814716795148684 ) ) ;
#10374 = CARTESIAN_POINT ( 'NONE',  ( -0.3766621274091715987, 0.5000000000000000000, -0.1347136637304948981 ) ) ;
#10375 = VERTEX_POINT ( 'NONE', #4409 ) ;
#10376 = ORIENTED_EDGE ( 'NONE', *, *, #8477, .F. ) ;
#10377 = CARTESIAN_POINT ( 'NONE',  ( 10.56600390958041302, 8.673617379884035472E-16, -167.0813103633617231 ) ) ;
#10378 = CARTESIAN_POINT ( 'NONE',  ( -3.749999999999999556, 2.312500000000000888, -5.053300858899104853 ) ) ;
#10379 = CARTESIAN_POINT ( 'NONE',  ( -3.749999999999999556, 0.7499999999999998890, -3.499999999999999112 ) ) ;
#10380 = CARTESIAN_POINT ( 'NONE',  ( -1.376260179405575323, 15.00000000000000000, -106.6458321843530541 ) ) ;
#10381 = ORIENTED_EDGE ( 'NONE', *, *, #7191, .T. ) ;
#10382 = CARTESIAN_POINT ( 'NONE',  ( -2.298097038856278918, 7.375000000000000888, -5.798097038856277585 ) ) ;
#10383 = CARTESIAN_POINT ( 'NONE',  ( -3.249999999999999556, 1.750000000000000000, -3.500000000000000000 ) ) ;
#10384 = B_SPLINE_CURVE_WITH_KNOTS ( 'NONE', 3,
 ( #2839, #8780, #439, #1666 ),
 .UNSPECIFIED., .F., .F.,
 ( 4, 4 ),
 ( 0.08237334560920292481, 0.08250179899282622520 ),
 .UNSPECIFIED. ) ;
#10385 = CIRCLE ( 'NONE', #5205, 4.999999999999998224 ) ;
#10386 = CARTESIAN_POINT ( 'NONE',  ( -48.64052431954574729, 14.99999999999769074, -142.5706416667350425 ) ) ;
#10387 = CIRCLE ( 'NONE', #10877, 0.9999999999999987788 ) ;
#10388 = AXIS2_PLACEMENT_3D ( 'NONE', #13370, #6552, #7708 ) ;
#10389 = CARTESIAN_POINT ( 'NONE',  ( -2.141054399116760543, 5.000000000000000000, -102.7251783244459631 ) ) ;
#10390 =( NAMED_UNIT ( * ) PLANE_ANGLE_UNIT ( ) SI_UNIT ( $, .RADIAN. ) );
#10391 = CARTESIAN_POINT ( 'NONE',  ( -3.249999999999999556, 4.187500000000000000, -2.153805922287440833 ) ) ;
#10392 = CONTEXT_DEPENDENT_SHAPE_REPRESENTATION ( #11918, #297 ) ;
#10393 = CARTESIAN_POINT ( 'NONE',  ( 26.71007981443199952, 6.000000000000000000, -136.8791680534710054 ) ) ;
#10394 = CARTESIAN_POINT ( 'NONE',  ( 38.25296960060453699, 0.000000000000000000, 42.65758570601131794 ) ) ;
#10395 = VERTEX_POINT ( 'NONE', #13848 ) ;
#10396 = CARTESIAN_POINT ( 'NONE',  ( 1.299830696487494386, 4.000000000000000000, -139.3994634862947635 ) ) ;
#10397 = CARTESIAN_POINT ( 'NONE',  ( 1.346194077712558279, 9.562500000000000000, -6.750000000000000000 ) ) ;
#10398 = CC_DESIGN_PERSON_AND_ORGANIZATION_ASSIGNMENT ( #11799, #15307, ( #10180 ) ) ;
#10399 = CIRCLE ( 'NONE', #5698, 1.771449424009377438 ) ;
#10400 = ORIENTED_EDGE ( 'NONE', *, *, #9491, .T. ) ;
#10401 = ORIENTED_EDGE ( 'NONE', *, *, #9597, .F. ) ;
#10402 = CARTESIAN_POINT ( 'NONE',  ( -4.592425496802573972E-16, 11.00000000000000000, -7.250000000000000000 ) ) ;
#10403 = CARTESIAN_POINT ( 'NONE',  ( 51.19063959271458231, 1.750000000000000000, 70.12932606827693860 ) ) ;
#10404 =( BOUNDED_SURFACE ( )  B_SPLINE_SURFACE ( 3, 1, ( 
 ( #11364, #639 ),
 ( #12603, #9051 ),
 ( #6505, #9982 ),
 ( #4121, #790 ) ),
 .UNSPECIFIED., .F., .F., .F. ) 
 B_SPLINE_SURFACE_WITH_KNOTS ( ( 4, 4 ),
 ( 2, 2 ),
 ( 0.000000000000000000, 1.000000000000000000 ),
 ( 0.000000000000000000, 1.000000000000000000 ),
 .UNSPECIFIED. ) 
 GEOMETRIC_REPRESENTATION_ITEM ( )  RATIONAL_B_SPLINE_SURFACE ( (
 ( 1.000000000000000000, 1.000000000000000000),
 ( 0.9216682375510407699, 0.9216682375510407699),
 ( 0.9216682375510407699, 0.9216682375510407699),
 ( 1.000000000000000000, 1.000000000000000000) ) ) 
 REPRESENTATION_ITEM ( '' )  SURFACE ( )  );
#10405 = CARTESIAN_POINT ( 'NONE',  ( 1.553300858899109516, 1.437500000000000000, 0.2499999999999993616 ) ) ;
#10406 = CARTESIAN_POINT ( 'NONE',  ( 2.298097038856278029, 7.125000000000000888, -5.798097038856279362 ) ) ;
#10407 = ORIENTED_EDGE ( 'NONE', *, *, #647, .T. ) ;
#10408 = CARTESIAN_POINT ( 'NONE',  ( 22.39039888797916333, 1.750000000000027756, 68.66652033670405331 ) ) ;
#10409 = CARTESIAN_POINT ( 'NONE',  ( 0.000000000000000000, 2.000000000000000000, -0.2500000000000002220 ) ) ;
#10410 = CARTESIAN_POINT ( 'NONE',  ( -3.749999999999999556, 7.187500000000000000, -1.946699141100892927 ) ) ;
#10411 = CARTESIAN_POINT ( 'NONE',  ( -25.21522606501703834, 1.851995413243205713, -207.7825160301809149 ) ) ;
#10412 = FACE_OUTER_BOUND ( 'NONE', #10477, .T. ) ;
#10413 = APPROVAL_STATUS ( 'not_yet_approved' ) ;
#10414 = CARTESIAN_POINT ( 'NONE',  ( 26.71007981443199952, 5.000000000000000888, -136.8791680534710054 ) ) ;
#10415 = ORIENTED_EDGE ( 'NONE', *, *, #6650, .T. ) ;
#10416 = CARTESIAN_POINT ( 'NONE',  ( 3.249999999999998224, 9.187500000000001776, -4.846194077712561388 ) ) ;
#10417 = PRODUCT_DEFINITION_FORMATION_WITH_SPECIFIED_SOURCE ( 'ANY', '', #6227, .NOT_KNOWN. ) ;
#10418 = CARTESIAN_POINT ( 'NONE',  ( 10.97402408521754857, 13.16001484901744334, -107.0745672077283785 ) ) ;
#10419 = CARTESIAN_POINT ( 'NONE',  ( 2.651650429449552870, 9.125000000000001776, -6.151650429449553314 ) ) ;
#10420 = CARTESIAN_POINT ( 'NONE',  ( 1.553300858899105963, 13.56250000000000000, -7.250000000000000000 ) ) ;
#10421 = CARTESIAN_POINT ( 'NONE',  ( -64.43123794286421457, 13.62327337436093799, -200.0781115302953310 ) ) ;
#10422 = LINE ( 'NONE', #3459, #8405 ) ;
#10423 = CARTESIAN_POINT ( 'NONE',  ( -4.592425496802573972E-16, 14.00000000000000000, -7.250000000000000000 ) ) ;
#10424 = CARTESIAN_POINT ( 'NONE',  ( -8.871427270046806868, 4.336808689942020694E-16, -127.2226661771092040 ) ) ;
#10425 = COORDINATED_UNIVERSAL_TIME_OFFSET ( 0, 0, .AHEAD. ) ;
#10426 = LOCAL_TIME ( 12, 28, 20.00000000000000000, #5089 ) ;
#10427 = DIRECTION ( 'NONE',  ( 0.000000000000000000, 0.000000000000000000, 1.000000000000000000 ) ) ;
#10428 = EDGE_LOOP ( 'NONE', ( #2844, #7004, #9849, #12518, #6836 ) ) ;
#10429 = CARTESIAN_POINT ( 'NONE',  ( 6.052559506676158385, 3.990476221019045866, 5.174528079217774135 ) ) ;
#10430 = CARTESIAN_POINT ( 'NONE',  ( 0.000000000000000000, 3.000000000000000000, -0.2500000000000002220 ) ) ;
#10431 = CIRCLE ( 'NONE', #11174, 6.999999999999950262 ) ;
#10432 = CARTESIAN_POINT ( 'NONE',  ( -61.24268700630520357, 15.00000000000266986, -190.3758570956361211 ) ) ;
#10433 = CARTESIAN_POINT ( 'NONE',  ( -3.249999999999999112, 2.812500000000000444, -4.846194077712558723 ) ) ;
#10434 = ORIENTED_EDGE ( 'NONE', *, *, #3371, .T. ) ;
#10435 = CARTESIAN_POINT ( 'NONE',  ( 51.62524086895221842, 0.000000000000000000, 69.88209797381232136 ) ) ;
#10436 = CARTESIAN_POINT ( 'NONE',  ( 1.831246893856137481, 2.490287375297123074, -1.000000000000007772 ) ) ;
#10437 = CARTESIAN_POINT ( 'NONE',  ( 8.957191258107528142, 11.99542373187157018, 1.863686112684491025 ) ) ;
#10438 = EDGE_CURVE ( 'NONE', #14605, #4391, #7960, .T. ) ;
#10439 = CARTESIAN_POINT ( 'NONE',  ( 5.000000000000000000, 8.673617379884035472E-16, -100.6237003951525537 ) ) ;
#10440 = CARTESIAN_POINT ( 'NONE',  ( 0.000000000000000000, 12.50000000000000178, -0.2500000000000002220 ) ) ;
#10441 = CARTESIAN_POINT ( 'NONE',  ( 3.136841903360915396, 15.00000000000000000, -104.4936450199714955 ) ) ;
#10442 = CARTESIAN_POINT ( 'NONE',  ( -3.750000000000000000, 0.8125000000000001110, -5.053300858899105741 ) ) ;
#10443 = VECTOR ( 'NONE', #7863, 1000.000000000000000 ) ;
#10444 = CARTESIAN_POINT ( 'NONE',  ( -1.990360824022270991, 6.321094445766561876, -22.54485386122858515 ) ) ;
#10445 = DIRECTION ( 'NONE',  ( -0.9997619372588932851, -0.000000000000000000, -0.02181900108494707474 ) ) ;
#10446 = CARTESIAN_POINT ( 'NONE',  ( 6.369258321017759350, 2.075239479414269894, -34.56909192082981974 ) ) ;
#10447 = CARTESIAN_POINT ( 'NONE',  ( -1.489212485369225458, 2.100000000000000089, -1.373268335280311891 ) ) ;
#10448 = CARTESIAN_POINT ( 'NONE',  ( 1.346194077712558057, 7.562500000000000000, -6.750000000000000000 ) ) ;
#10449 = DIRECTION ( 'NONE',  ( -0.000000000000000000, -1.000000000000000000, -0.000000000000000000 ) ) ;
#10450 = CARTESIAN_POINT ( 'NONE',  ( -12.27209645382209402, 9.999999999999998224, -127.2227734861304782 ) ) ;
#10451 = VERTEX_POINT ( 'NONE', #1008 ) ;
#10452 = ORIENTED_EDGE ( 'NONE', *, *, #4512, .T. ) ;
#10453 = CARTESIAN_POINT ( 'NONE',  ( 10.73212172315381885, 12.50000000000000533, -107.4514619188133082 ) ) ;
#10454 = CARTESIAN_POINT ( 'NONE',  ( -1.553300858899106629, 4.062500000000000000, 0.2500000000000002220 ) ) ;
#10455 = VECTOR ( 'NONE', #3102, 1000.000000000000000 ) ;
#10456 = CARTESIAN_POINT ( 'NONE',  ( 1.553300858899105963, 2.062500000000000000, -7.249999999999999112 ) ) ;
#10457 = CIRCLE ( 'NONE', #12428, 3.250000000000005329 ) ;
#10458 = CARTESIAN_POINT ( 'NONE',  ( 26.64011553632023066, 4.666487833696466581, -138.9157185642569914 ) ) ;
#10459 = VERTEX_POINT ( 'NONE', #10436 ) ;
#10460 = CARTESIAN_POINT ( 'NONE',  ( 0.000000000000000000, 14.00000000000000000, -0.2500000000000002220 ) ) ;
#10461 = EDGE_CURVE ( 'NONE', #6301, #11483, #12486, .T. ) ;
#10462 = EDGE_CURVE ( 'NONE', #7347, #14600, #842, .T. ) ;
#10463 = CARTESIAN_POINT ( 'NONE',  ( -1.346194077712559389, 11.43750000000000000, -6.749999999999999112 ) ) ;
#10464 = CARTESIAN_POINT ( 'NONE',  ( -2.397620167341370845, 5.000000000000000888, -107.6176329143618062 ) ) ;
#10465 =( LENGTH_UNIT ( ) NAMED_UNIT ( * ) SI_UNIT ( .MILLI., .METRE. ) );
#10466 = CC_DESIGN_PERSON_AND_ORGANIZATION_ASSIGNMENT ( #1804, #11432, ( #10417 ) ) ;
#10467 = CARTESIAN_POINT ( 'NONE',  ( 0.000000000000000000, 4.000000000000000000, -0.2500000000000002220 ) ) ;
#10468 = AXIS2_PLACEMENT_3D ( 'NONE', #12834, #11443, #2021 ) ;
#10469 = APPROVAL_STATUS ( 'not_yet_approved' ) ;
#10470 = AXIS2_PLACEMENT_3D ( 'NONE', #13701, #8897, #8823 ) ;
#10471 = DIRECTION ( 'NONE',  ( 0.000000000000000000, 0.000000000000000000, -1.000000000000000000 ) ) ;
#10472 = DIRECTION ( 'NONE',  ( -0.000000000000000000, -1.000000000000000000, -0.000000000000000000 ) ) ;
#10473 = EDGE_LOOP ( 'NONE', ( #6889, #4321, #7345, #2073 ) ) ;
#10474 = CARTESIAN_POINT ( 'NONE',  ( 2.547208780220832747, -1.831210392890420424, -1.000000000000001332 ) ) ;
#10475 = CARTESIAN_POINT ( 'NONE',  ( 0.000000000000000000, 13.00000000000000178, -0.2500000000000002220 ) ) ;
#10476 = ORIENTED_EDGE ( 'NONE', *, *, #3712, .T. ) ;
#10477 = EDGE_LOOP ( 'NONE', ( #4336, #2113 ) ) ;
#10478 = CARTESIAN_POINT ( 'NONE',  ( -1.553300858899106629, 8.562500000000000000, 0.2500000000000002220 ) ) ;
#10479 = CARTESIAN_POINT ( 'NONE',  ( 37.88191578704504536, 0.000000000000000000, 42.20832867525968624 ) ) ;
#10480 = CARTESIAN_POINT ( 'NONE',  ( 3.750000000000000000, 7.312500000000001776, -1.946699141100892705 ) ) ;
#10481 = CARTESIAN_POINT ( 'NONE',  ( -1.346194077712559167, 7.937500000000001776, -6.749999999999999112 ) ) ;
#10482 = EDGE_LOOP ( 'NONE', ( #11685, #14378, #14794, #403 ) ) ;
#10483 = CARTESIAN_POINT ( 'NONE',  ( 6.153839613028314837, 12.51224853425506289, 4.615052189839248697 ) ) ;
#10484 = CONICAL_SURFACE ( 'NONE', #1602, 0.5000000000000018874, 0.6283185307179600665 ) ;
#10485 = CARTESIAN_POINT ( 'NONE',  ( 3.249999999999999112, 1.812500000000000222, -2.153805922287439945 ) ) ;
#10486 = EDGE_CURVE ( 'NONE', #9776, #14605, #13928, .T. ) ;
#10487 = PRODUCT_DEFINITION ( 'UNKNOWN', '', #12090, #1704 ) ;
#10488 = CARTESIAN_POINT ( 'NONE',  ( -3.749999999999999556, 4.187500000000000000, -1.946699141100892927 ) ) ;
#10489 = CIRCLE ( 'NONE', #7769, 0.5000000000000000000 ) ;
#10490 = CARTESIAN_POINT ( 'NONE',  ( -25.70029544500438590, 0.7328807590276666950, -204.7564699162097099 ) ) ;
#10491 = CARTESIAN_POINT ( 'NONE',  ( -17.32624372123753886, 2.500000000000000444, -122.3796757791585321 ) ) ;
#10492 = MECHANICAL_CONTEXT ( 'NONE', #7975, 'mechanical' ) ;
#10493 = DIRECTION ( 'NONE',  ( -0.000000000000000000, -1.000000000000000000, -0.000000000000000000 ) ) ;
#10494 =( BOUNDED_SURFACE ( )  B_SPLINE_SURFACE ( 3, 1, ( 
 ( #12596, #10126 ),
 ( #3241, #860 ),
 ( #6497, #4404 ),
 ( #9113, #15088 ) ),
 .UNSPECIFIED., .F., .F., .T. ) 
 B_SPLINE_SURFACE_WITH_KNOTS ( ( 4, 4 ),
 ( 2, 2 ),
 ( 0.000000000000000000, 1.000000000000000000 ),
 ( 0.000000000000000000, 1.000000000000000000 ),
 .UNSPECIFIED. ) 
 GEOMETRIC_REPRESENTATION_ITEM ( )  RATIONAL_B_SPLINE_SURFACE ( (
 ( 1.000000000000000000, 1.000000000000000000),
 ( 0.6468719831415924437, 0.6468719831415924437),
 ( 0.6468719831415924437, 0.6468719831415924437),
 ( 1.000000000000000000, 1.000000000000000000) ) ) 
 REPRESENTATION_ITEM ( '' )  SURFACE ( )  );
#10495 = EDGE_LOOP ( 'NONE', ( #11012, #3099, #3529, #9609 ) ) ;
#10496 = CARTESIAN_POINT ( 'NONE',  ( -3.249999999999999556, 5.750000000000000000, -3.500000000000000000 ) ) ;
#10497 = LINE ( 'NONE', #15229, #1305 ) ;
#10498 = CARTESIAN_POINT ( 'NONE',  ( -2.651650429449552870, 10.87500000000000000, -6.151650429449552426 ) ) ;
#10499 = CARTESIAN_POINT ( 'NONE',  ( -3.750000000000000000, 13.18750000000000000, -1.946699141100892927 ) ) ;
#10500 = CARTESIAN_POINT ( 'NONE',  ( -65.88169384473235368, 15.09374676575395924, -201.3968192357596934 ) ) ;
#10501 = CARTESIAN_POINT ( 'NONE',  ( -6.371526220232841098, 5.000000000000000888, -125.9870988568622465 ) ) ;
#10502 = CARTESIAN_POINT ( 'NONE',  ( 3.750000000000000000, 14.31250000000000355, -1.946699141100892705 ) ) ;
#10503 = DIRECTION ( 'NONE',  ( -8.673617379884027583E-16, 0.000000000000000000, -1.000000000000000000 ) ) ;
#10504 = DATE_AND_TIME ( #11578, #10916 ) ;
#10505 = CARTESIAN_POINT ( 'NONE',  ( 11.06771612204629207, 8.749999999999998224, -94.84204383295364948 ) ) ;
#10506 = ORIENTED_EDGE ( 'NONE', *, *, #45, .T. ) ;
#10507 = CARTESIAN_POINT ( 'NONE',  ( -25.49544145210780499, 8.673617379884035472E-16, -197.0346082499829095 ) ) ;
#10508 = CARTESIAN_POINT ( 'NONE',  ( -3.980102097228897245E-16, 2.500000000000000000, -6.749999999999999112 ) ) ;
#10509 = CARTESIAN_POINT ( 'NONE',  ( -67.64066136719213773, 14.99999999999999822, -197.5793268429668217 ) ) ;
#10510 = CARTESIAN_POINT ( 'NONE',  ( 3.249999999999998224, 1.312500000000000444, -2.153805922287439945 ) ) ;
#10511 = ORIENTED_EDGE ( 'NONE', *, *, #11272, .T. ) ;
#10512 = CARTESIAN_POINT ( 'NONE',  ( 1.077013294873430338, -2.254417391461207565, -1.000000000000001110 ) ) ;
#10513 = CARTESIAN_POINT ( 'NONE',  ( -25.64914917419623208, 1.594688008273111635, -206.8106692875541910 ) ) ;
#10514 = CARTESIAN_POINT ( 'NONE',  ( 8.973073561997775727, 12.37582002200307585, 1.135947805892676410 ) ) ;
#10515 = FACE_BOUND ( 'NONE', #13098, .T. ) ;
#10516 = CARTESIAN_POINT ( 'NONE',  ( -3.249999999999999556, 10.75000000000000178, -3.500000000000000000 ) ) ;
#10517 = CARTESIAN_POINT ( 'NONE',  ( 26.15341798802279527, 4.000000000000000000, -138.2600702976168350 ) ) ;
#10518 = CARTESIAN_POINT ( 'NONE',  ( 3.750000000000000000, 0.3125000000000002220, -1.946699141100892705 ) ) ;
#10519 = DIRECTION ( 'NONE',  ( 1.000000000000000000, 0.000000000000000000, 0.000000000000000000 ) ) ;
#10520 = CARTESIAN_POINT ( 'NONE',  ( -3.797473941148798104, 10.19338465826168516, -43.01405755766484162 ) ) ;
#10521 = EDGE_CURVE ( 'NONE', #10617, #3600, #8419, .T. ) ;
#10522 = CARTESIAN_POINT ( 'NONE',  ( -6.563559844847487668, 10.00000000000000178, -119.2393675976817491 ) ) ;
#10523 = EDGE_CURVE ( 'NONE', #11692, #5961, #5124, .T. ) ;
#10524 = CARTESIAN_POINT ( 'NONE',  ( -3.125658737029940681, 0.000000000000000000, 3.587914672538146554 ) ) ;
#10525 = CARTESIAN_POINT ( 'NONE',  ( 1.346194077712558057, 13.56250000000000000, -6.750000000000000000 ) ) ;
#10526 = LINE ( 'NONE', #15259, #9887 ) ;
#10527 = CARTESIAN_POINT ( 'NONE',  ( -64.50864733187511035, 13.73033652205686472, -199.7707221509654403 ) ) ;
#10528 = EDGE_LOOP ( 'NONE', ( #11513, #11702, #1272, #5975 ) ) ;
#10529 = ORIENTED_EDGE ( 'NONE', *, *, #1488, .F. ) ;
#10530 = CARTESIAN_POINT ( 'NONE',  ( 14.22910372453204353, 6.000000000000000000, -126.5134921567817941 ) ) ;
#10531 = CARTESIAN_POINT ( 'NONE',  ( 2.651650429449552870, 3.625000000000000000, -6.151650429449554203 ) ) ;
#10532 = CARTESIAN_POINT ( 'NONE',  ( 3.749999999999999556, 5.249999999999999112, -3.500000000000000444 ) ) ;
#10533 = CARTESIAN_POINT ( 'NONE',  ( 9.939878312292631080, 15.00000000000000888, -115.2320631035898657 ) ) ;
#10534 = ORIENTED_EDGE ( 'NONE', *, *, #4512, .F. ) ;
#10535 = CARTESIAN_POINT ( 'NONE',  ( 1.346194077712558057, 13.56250000000000000, -6.750000000000000000 ) ) ;
#10536 = CARTESIAN_POINT ( 'NONE',  ( -5.082498805844318568, 5.000000000000001776, -111.2070015758558696 ) ) ;
#10537 = CARTESIAN_POINT ( 'NONE',  ( 42.09231163430414568, 0.000000000000000000, 51.87369981213807080 ) ) ;
#10538 = CARTESIAN_POINT ( 'NONE',  ( 3.249999999999999556, 5.750000000000000000, -3.500000000000000000 ) ) ;
#10539 = SECURITY_CLASSIFICATION_LEVEL ( 'unclassified' ) ;
#10540 = EDGE_CURVE ( 'NONE', #11406, #10699, #11207, .T. ) ;
#10541 = DIRECTION ( 'NONE',  ( 0.000000000000000000, -1.000000000000000000, 0.000000000000000000 ) ) ;
#10542 = CARTESIAN_POINT ( 'NONE',  ( 25.37357285188495837, -5.098721647816789303E-12, -136.0302139099745773 ) ) ;
#10543 = ORIENTED_EDGE ( 'NONE', *, *, #10749, .T. ) ;
#10544 = ADVANCED_FACE ( 'NONE', ( #8491 ), #9654, .F. ) ;
#10545 = PLANE ( 'NONE',  #7909 ) ;
#10546 = CARTESIAN_POINT ( 'NONE',  ( 1.346194077712558279, 10.56250000000000000, -6.750000000000000000 ) ) ;
#10547 = ORIENTED_EDGE ( 'NONE', *, *, #1292, .T. ) ;
#10548 = VERTEX_POINT ( 'NONE', #12126 ) ;
#10549 = DIRECTION ( 'NONE',  ( -1.000000000000000000, -0.000000000000000000, -0.000000000000000000 ) ) ;
#10550 = CARTESIAN_POINT ( 'NONE',  ( 3.749999999999999556, 4.250000000000000000, -3.500000000000000444 ) ) ;
#10551 = CARTESIAN_POINT ( 'NONE',  ( -1.346194077712559167, 6.937500000000001776, -6.749999999999999112 ) ) ;
#10552 = ORIENTED_EDGE ( 'NONE', *, *, #7140, .F. ) ;
#10553 = CARTESIAN_POINT ( 'NONE',  ( 8.673617379884035472E-16, 14.99999999999999645, -100.6237003951525679 ) ) ;
#10554 = CARTESIAN_POINT ( 'NONE',  ( -3.249999999999999556, 4.250000000000000000, -3.499999999999999556 ) ) ;
#10555 = CARTESIAN_POINT ( 'NONE',  ( -3.749999999999999556, 10.18750000000000000, -1.946699141100892927 ) ) ;
#10556 = CARTESIAN_POINT ( 'NONE',  ( -25.49686867869201023, 0.3475987381038808111, -203.6525958643808281 ) ) ;
#10557 = FACE_OUTER_BOUND ( 'NONE', #5623, .T. ) ;
#10558 = CARTESIAN_POINT ( 'NONE',  ( 0.3766621274091715987, 0.5000000000000000000, 0.1491815183709511716 ) ) ;
#10559 = APPROVAL_STATUS ( 'not_yet_approved' ) ;
#10560 = CARTESIAN_POINT ( 'NONE',  ( 3.717577911061872520, 5.000000000000000888, -143.6771719914432595 ) ) ;
#10561 = EDGE_CURVE ( 'NONE', #5120, #13895, #11936, .T. ) ;
#10562 = ORIENTED_EDGE ( 'NONE', *, *, #13590, .T. ) ;
#10563 = CARTESIAN_POINT ( 'NONE',  ( 2.298097038856279362, 8.375000000000000000, -1.201902961143720860 ) ) ;
#10564 = CARTESIAN_POINT ( 'NONE',  ( -2.651650429449552870, 7.625000000000000000, -0.8483495705504467965 ) ) ;
#10565 = CARTESIAN_POINT ( 'NONE',  ( 9.044950117654433797, -4.000000000000000000, -141.4826476090360643 ) ) ;
#10566 = CARTESIAN_POINT ( 'NONE',  ( -65.15039301591723131, 14.86702644047977451, -190.2334373523178783 ) ) ;
#10567 = CARTESIAN_POINT ( 'NONE',  ( -1.362135537567234378, 1.125083754270053138, -137.9888685449287777 ) ) ;
#10568 = CARTESIAN_POINT ( 'NONE',  ( 2.651650429449552870, 14.12500000000000000, -6.151650429449555091 ) ) ;
#10569 = FACE_BOUND ( 'NONE', #1151, .T. ) ;
#10570 = PERSON_AND_ORGANIZATION ( #3176, #3020 ) ;
#10571 = CARTESIAN_POINT ( 'NONE',  ( 3.867493089945844620, 14.96835584425696730, -13.04672393183693480 ) ) ;
#10572 = CARTESIAN_POINT ( 'NONE',  ( 1.081679185590002756, 4.727159810604965706, -139.4347531963001643 ) ) ;
#10573 = ORIENTED_EDGE ( 'NONE', *, *, #7100, .F. ) ;
#10574 = CARTESIAN_POINT ( 'NONE',  ( -25.15829320847776529, -1.662059052993006175E-12, -208.1809449273558528 ) ) ;
#10575 = CARTESIAN_POINT ( 'NONE',  ( 0.000000000000000000, 5.000000000000000000, -0.2500000000000002220 ) ) ;
#10576 = CARTESIAN_POINT ( 'NONE',  ( -6.683304552674631971, 4.336808689942017736E-16, -104.1296019027812463 ) ) ;
#10577 = CARTESIAN_POINT ( 'NONE',  ( -1.346194077712558945, 6.562500000000000888, -0.2500000000000002220 ) ) ;
#10578 = VERTEX_POINT ( 'NONE', #4789 ) ;
#10579 = CARTESIAN_POINT ( 'NONE',  ( -1.535122803310335238, 15.00000000000000000, -120.1898458067378641 ) ) ;
#10580 = CARTESIAN_POINT ( 'NONE',  ( 2.321679137609549137, 14.14938758934379237, 1.340907874341730199 ) ) ;
#10581 = CARTESIAN_POINT ( 'NONE',  ( -11.91260474553833504, 15.00000000000000000, -150.3549708559484088 ) ) ;
#10582 = CARTESIAN_POINT ( 'NONE',  ( 3.249999999999998668, 1.687500000000000000, -4.846194077712560500 ) ) ;
#10583 = CARTESIAN_POINT ( 'NONE',  ( -3.249999999999999556, 12.75000000000000178, -3.500000000000000000 ) ) ;
#10584 = DIRECTION ( 'NONE',  ( -0.000000000000000000, -1.000000000000000000, -0.000000000000000000 ) ) ;
#10585 = CARTESIAN_POINT ( 'NONE',  ( -4.592425496802573972E-16, 3.000000000000000444, -7.250000000000000000 ) ) ;
#10586 = LINE ( 'NONE', #12920, #13180 ) ;
#10587 = CARTESIAN_POINT ( 'NONE',  ( 16.45731177154546998, 8.749999999999998224, -89.72322964069195450 ) ) ;
#10588 = CARTESIAN_POINT ( 'NONE',  ( 1.004809442601929836, 5.666666666666666963, -139.4752805618705622 ) ) ;
#10589 = CARTESIAN_POINT ( 'NONE',  ( 3.481334635432024260, 11.96985545825839914, 4.757046313331589005 ) ) ;
#10590 = CARTESIAN_POINT ( 'NONE',  ( -3.980102097228897245E-16, 12.50000000000000000, -6.749999999999999112 ) ) ;
#10591 = DIRECTION ( 'NONE',  ( 0.000000000000000000, 0.000000000000000000, -1.000000000000000000 ) ) ;
#10592 = CARTESIAN_POINT ( 'NONE',  ( 0.7552767017676234040, 8.673617379884035472E-16, -110.7727649483481400 ) ) ;
#10593 = VERTEX_POINT ( 'NONE', #10737 ) ;
#10594 = CC_DESIGN_SECURITY_CLASSIFICATION ( #4203, ( #10116 ) ) ;
#10595 = ORIENTED_EDGE ( 'NONE', *, *, #9967, .T. ) ;
#10596 = CARTESIAN_POINT ( 'NONE',  ( -5.223664414429025626, 3.333353350040314295E-13, -111.8183263698978607 ) ) ;
#10597 = CARTESIAN_POINT ( 'NONE',  ( 8.364153288505452366, 12.49999999999999645, -112.7786105982117419 ) ) ;
#10598 = CARTESIAN_POINT ( 'NONE',  ( 2.651650429449552870, 6.625000000000000000, -6.151650429449554203 ) ) ;
#10599 = CARTESIAN_POINT ( 'NONE',  ( 3.749999999999999112, 4.312500000000000000, -1.946699141100893149 ) ) ;
#10600 = AXIS2_PLACEMENT_3D ( 'NONE', #12716, #4668, #9608 ) ;
#10601 = CARTESIAN_POINT ( 'NONE',  ( 8.595858757335200551, 15.00000000000202860, -113.5677547687581779 ) ) ;
#10602 = ORIENTED_EDGE ( 'NONE', *, *, #468, .T. ) ;
#10603 = CARTESIAN_POINT ( 'NONE',  ( 1.346194077712561166, 2.437500000000000444, -0.2500000000000011102 ) ) ;
#10604 = DIRECTION ( 'NONE',  ( -0.000000000000000000, -0.000000000000000000, -1.000000000000000000 ) ) ;
#10605 = LOCAL_TIME ( 12, 28, 20.00000000000000000, #15148 ) ;
#10606 = DIRECTION ( 'NONE',  ( 0.000000000000000000, 0.000000000000000000, 1.000000000000000000 ) ) ;
#10607 = CARTESIAN_POINT ( 'NONE',  ( 2.298097038856278473, 2.625000000000000000, -5.798097038856279362 ) ) ;
#10608 = AXIS2_PLACEMENT_3D ( 'NONE', #10389, #11397, #1037 ) ;
#10609 = EDGE_CURVE ( 'NONE', #7526, #11904, #13390, .T. ) ;
#10610 = APPROVAL_STATUS ( 'not_yet_approved' ) ;
#10611 = DIRECTION ( 'NONE',  ( 0.000000000000000000, 0.000000000000000000, -1.000000000000000000 ) ) ;
#10612 = CARTESIAN_POINT ( 'NONE',  ( 12.21230042287087691, 5.000000000000000888, -124.0782217030330656 ) ) ;
#10613 = EDGE_LOOP ( 'NONE', ( #9646, #12312, #14907, #11063 ) ) ;
#10614 = DIRECTION ( 'NONE',  ( -8.764770998266002131E-18, 0.000000000000000000, -1.000000000000000000 ) ) ;
#10615 = CARTESIAN_POINT ( 'NONE',  ( 2.298097038856278473, 13.62500000000000000, -5.798097038856279362 ) ) ;
#10616 = EDGE_LOOP ( 'NONE', ( #6888, #1505, #6755, #9255 ) ) ;
#10617 = VERTEX_POINT ( 'NONE', #8409 ) ;
#10618 = CARTESIAN_POINT ( 'NONE',  ( -3.384109865120556560, 2.331468351712828340E-16, 30.80069534665370767 ) ) ;
#10619 = CARTESIAN_POINT ( 'NONE',  ( 0.000000000000000000, 5.500000000000000888, 0.2500000000000002220 ) ) ;
#10620 = CARTESIAN_POINT ( 'NONE',  ( 2.298097038856279362, 7.375000000000000000, -1.201902961143720860 ) ) ;
#10621 = ORIENTED_EDGE ( 'NONE', *, *, #317, .F. ) ;
#10622 = LOCAL_TIME ( 12, 28, 20.00000000000000000, #11400 ) ;
#10623 = CARTESIAN_POINT ( 'NONE',  ( 6.321864114638128918, 14.74656758735381779, 1.877230377063963784 ) ) ;
#10624 = CARTESIAN_POINT ( 'NONE',  ( 3.249999999999999112, 2.812500000000000000, -2.153805922287439945 ) ) ;
#10625 = CIRCLE ( 'NONE', #9879, 8.000000000000007105 ) ;
#10626 = VECTOR ( 'NONE', #4852, 1000.000000000000114 ) ;
#10627 = EDGE_CURVE ( 'NONE', #6698, #4658, #1579, .T. ) ;
#10628 = LINE ( 'NONE', #1437, #4441 ) ;
#10629 = DIRECTION ( 'NONE',  ( -0.9961255586397056438, 0.000000000000000000, 0.08794243244722428632 ) ) ;
#10630 = CARTESIAN_POINT ( 'NONE',  ( -5.488578029460351893, -2.529993217055220178, -43.69424231201529096 ) ) ;
#10631 = PERSON_AND_ORGANIZATION ( #3176, #3020 ) ;
#10632 = VECTOR ( 'NONE', #7595, 1000.000000000000000 ) ;
#10633 = CARTESIAN_POINT ( 'NONE',  ( -61.77944655731723600, 14.99999999999999822, -173.7574396188045114 ) ) ;
#10634 = VECTOR ( 'NONE', #13496, 1000.000000000000000 ) ;
#10635 = AXIS2_PLACEMENT_3D ( 'NONE', #6569, #11353, #7727 ) ;
#10636 = VERTEX_POINT ( 'NONE', #9503 ) ;
#10637 = CC_DESIGN_DATE_AND_TIME_ASSIGNMENT ( #10925, #1499, ( #12585 ) ) ;
#10638 = FACE_OUTER_BOUND ( 'NONE', #14035, .T. ) ;
#10639 = VECTOR ( 'NONE', #14823, 1000.000000000000227 ) ;
#10640 = EDGE_CURVE ( 'NONE', #2112, #1425, #1461, .T. ) ;
#10641 = CARTESIAN_POINT ( 'NONE',  ( 2.651650429449552870, 13.12500000000000178, -6.151650429449553314 ) ) ;
#10642 = EDGE_CURVE ( 'NONE', #14924, #6350, #14175, .T. ) ;
#10643 = CARTESIAN_POINT ( 'NONE',  ( 0.000000000000000000, 1.000000000000000000, 0.000000000000000000 ) ) ;
#10644 = EDGE_CURVE ( 'NONE', #7777, #745, #10963, .T. ) ;
#10645 = CARTESIAN_POINT ( 'NONE',  ( -67.58911133235071134, 10.63074368436302741, -204.4236580053128023 ) ) ;
#10646 = DIRECTION ( 'NONE',  ( 0.000000000000000000, 0.000000000000000000, 1.000000000000000000 ) ) ;
#10647 = CARTESIAN_POINT ( 'NONE',  ( 2.298097038856278029, 3.125000000000000444, -5.798097038856279362 ) ) ;
#10648 = CARTESIAN_POINT ( 'NONE',  ( 10.03945249976937859, 1.886766667216011495, -106.6275678995573060 ) ) ;
#10649 = APPLICATION_PROTOCOL_DEFINITION ( 'international standard', 'config_control_design', 1994, #879 ) ;
#10650 = PRODUCT_DEFINITION_SHAPE ( 'NONE', 'NONE',  #2984 ) ;
#10651 = CARTESIAN_POINT ( 'NONE',  ( -29.69515346086419427, 10.00000000000000178, -156.7390981038714983 ) ) ;
#10652 = CARTESIAN_POINT ( 'NONE',  ( -16.31428614604211091, 0.05127365841283874903, -131.2397266576497543 ) ) ;
#10653 = APPROVAL ( #2842, 'UNSPECIFIED' ) ;
#10654 = VERTEX_POINT ( 'NONE', #7089 ) ;
#10655 = CARTESIAN_POINT ( 'NONE',  ( 8.358184211585273360, 2.650800484095609200, 2.505650865491267254 ) ) ;
#10656 = CARTESIAN_POINT ( 'NONE',  ( -1.346194077712559167, 1.437500000000000000, -6.749999999999999112 ) ) ;
#10657 = CARTESIAN_POINT ( 'NONE',  ( -51.02532656527229449, 14.99999999999733724, -166.3766172519595727 ) ) ;
#10658 = CARTESIAN_POINT ( 'NONE',  ( -1.346194077712559167, 6.937500000000001776, -6.749999999999999112 ) ) ;
#10659 = ORIENTED_EDGE ( 'NONE', *, *, #3836, .F. ) ;
#10660 = CARTESIAN_POINT ( 'NONE',  ( -0.3098342781321086759, 15.00000000000000000, -115.8337115950633063 ) ) ;
#10661 = CARTESIAN_POINT ( 'NONE',  ( -2.141054399116760543, 0.000000000000000000, -102.7251783244459631 ) ) ;
#10662 = CARTESIAN_POINT ( 'NONE',  ( -8.272624645314563097, 15.00000000000000000, -140.4230430975476054 ) ) ;
#10663 = DIRECTION ( 'NONE',  ( 0.000000000000000000, -1.000000000000000000, 0.000000000000000000 ) ) ;
#10664 = CARTESIAN_POINT ( 'NONE',  ( 3.249999999999998224, 15.31250000000000355, -2.153805922287439945 ) ) ;
#10665 = CARTESIAN_POINT ( 'NONE',  ( 1.553300858899105963, 4.562500000000001776, -7.250000000000000000 ) ) ;
#10666 = PRODUCT_DEFINITION_FORMATION_WITH_SPECIFIED_SOURCE ( 'ANY', '', #8304, .NOT_KNOWN. ) ;
#10667 = CARTESIAN_POINT ( 'NONE',  ( 0.1262058122322286813, 0.3029806520654600432, -7.146945437571384119 ) ) ;
#10668 = CARTESIAN_POINT ( 'NONE',  ( -3.749999999999999556, 3.750000000000000444, -3.499999999999999112 ) ) ;
#10669 = CARTESIAN_POINT ( 'NONE',  ( 0.5436898071449285386, 11.71486000072444433, 2.780856639695837185 ) ) ;
#10670 = CARTESIAN_POINT ( 'NONE',  ( -4.103993793088339892, 10.80977419301392928, -47.22237253197440765 ) ) ;
#10671 = CARTESIAN_POINT ( 'NONE',  ( 15.09707649861359613, 4.000000000000000000, -161.4544678506381388 ) ) ;
#10672 = CARTESIAN_POINT ( 'NONE',  ( -7.059949148491517334, 2.099999999999999645, 11.00002213459155875 ) ) ;
#10673 = CARTESIAN_POINT ( 'NONE',  ( -3.249999999999999556, 13.25000000000000000, -3.499999999999999556 ) ) ;
#10674 = DIRECTION ( 'NONE',  ( 0.000000000000000000, -1.000000000000000000, 0.000000000000000000 ) ) ;
#10675 = DIRECTION ( 'NONE',  ( -0.000000000000000000, 0.000000000000000000, 1.000000000000000000 ) ) ;
#10676 = ORIENTED_EDGE ( 'NONE', *, *, #5371, .T. ) ;
#10677 = VERTEX_POINT ( 'NONE', #11810 ) ;
#10678 = CARTESIAN_POINT ( 'NONE',  ( -5.248276757888013400, 2.500000000000000444, -115.0315526420553738 ) ) ;
#10679 = CARTESIAN_POINT ( 'NONE',  ( 11.04730217088350663, 12.49999999999999822, -107.1178495010082941 ) ) ;
#10680 = CARTESIAN_POINT ( 'NONE',  ( 3.749999999999998668, 6.687500000000000888, -5.053300858899107517 ) ) ;
#10681 = CARTESIAN_POINT ( 'NONE',  ( -4.592425496802573972E-16, 3.000000000000000444, -7.250000000000000000 ) ) ;
#10682 = CARTESIAN_POINT ( 'NONE',  ( 6.491365067585774362, 15.00000000000000000, 0.2705411889128706004 ) ) ;
#10683 = ORIENTED_EDGE ( 'NONE', *, *, #76, .F. ) ;
#10684 = VECTOR ( 'NONE', #11179, 1000.000000000000000 ) ;
#10685 = CARTESIAN_POINT ( 'NONE',  ( -3.249999999999999112, 3.812500000000000000, -4.846194077712558723 ) ) ;
#10686 = CARTESIAN_POINT ( 'NONE',  ( -51.71514206966925542, 14.99999999999999467, -145.7302012132438165 ) ) ;
#10687 = CARTESIAN_POINT ( 'NONE',  ( 26.15341798802279527, 4.000000000000000000, -138.7600702976168066 ) ) ;
#10688 = CARTESIAN_POINT ( 'NONE',  ( 0.000000000000000000, 6.000000000000000000, -0.2500000000000002220 ) ) ;
#10689 = CARTESIAN_POINT ( 'NONE',  ( -9.739626904459424139, 15.00000000000000178, -116.2879091882953446 ) ) ;
#10690 = CONTEXT_DEPENDENT_SHAPE_REPRESENTATION ( #13227, #9416 ) ;
#10691 = CARTESIAN_POINT ( 'NONE',  ( 26.15341798802279527, 6.000000000000000000, -138.7600702976168066 ) ) ;
#10692 = CARTESIAN_POINT ( 'NONE',  ( 11.09126156230712468, 2.140620105417839675E-13, -122.3351348873811162 ) ) ;
#10693 = ORIENTED_EDGE ( 'NONE', *, *, #13683, .F. ) ;
#10694 = VECTOR ( 'NONE', #13009, 1000.000000000000000 ) ;
#10695 = DIRECTION ( 'NONE',  ( -1.000000000000000000, 0.000000000000000000, 0.000000000000000000 ) ) ;
#10696 = AXIS2_PLACEMENT_3D ( 'NONE', #6864, #13918, #854 ) ;
#10697 = CARTESIAN_POINT ( 'NONE',  ( 1.346194077712558279, 14.56250000000000000, -6.750000000000000000 ) ) ;
#10698 = ORIENTED_EDGE ( 'NONE', *, *, #9151, .T. ) ;
#10699 = VERTEX_POINT ( 'NONE', #1227 ) ;
#10700 = DIRECTION ( 'NONE',  ( -0.000000000000000000, 1.000000000000000000, -0.000000000000000000 ) ) ;
#10701 = CARTESIAN_POINT ( 'NONE',  ( 1.553300858899109516, 4.437500000000001776, 0.2499999999999993616 ) ) ;
#10702 = CARTESIAN_POINT ( 'NONE',  ( -3.249999999999999112, 10.81250000000000000, -4.846194077712558723 ) ) ;
#10703 = VERTEX_POINT ( 'NONE', #10661 ) ;
#10704 = CARTESIAN_POINT ( 'NONE',  ( 3.167496085402304207, 15.00000000000000000, -107.8568673623673959 ) ) ;
#10705 = CARTESIAN_POINT ( 'NONE',  ( -2.298097038856278918, 2.375000000000000000, -5.798097038856277585 ) ) ;
#10706 = AXIS2_PLACEMENT_3D ( 'NONE', #9729, #612, #14460 ) ;
#10707 = AXIS2_PLACEMENT_3D ( 'NONE', #2019, #13927, #8107 ) ;
#10708 = DIRECTION ( 'NONE',  ( -0.000000000000000000, 1.000000000000000000, -0.000000000000000000 ) ) ;
#10709 = CARTESIAN_POINT ( 'NONE',  ( 12.03407860800352047, 1.493611570121361698, -165.3653928882239086 ) ) ;
#10710 =( BOUNDED_SURFACE ( )  B_SPLINE_SURFACE ( 3, 1, ( 
 ( #12026, #8712 ),
 ( #7387, #2535 ),
 ( #3770, #9558 ),
 ( #9637, #1296 ) ),
 .UNSPECIFIED., .F., .F., .T. ) 
 B_SPLINE_SURFACE_WITH_KNOTS ( ( 4, 4 ),
 ( 2, 2 ),
 ( 0.000000000000000000, 1.000000000000000000 ),
 ( 0.000000000000000000, 1.000000000000000000 ),
 .UNSPECIFIED. ) 
 GEOMETRIC_REPRESENTATION_ITEM ( )  RATIONAL_B_SPLINE_SURFACE ( (
 ( 1.000000000000000000, 1.000000000000000000),
 ( 0.8974116706346633165, 0.8974116706346633165),
 ( 0.8974116706346633165, 0.8974116706346633165),
 ( 1.000000000000000000, 1.000000000000000000) ) ) 
 REPRESENTATION_ITEM ( '' )  SURFACE ( )  );
#10711 = CARTESIAN_POINT ( 'NONE',  ( 6.293934161496127722, 14.99999999999999822, -117.6207956168515807 ) ) ;
#10712 = CALENDAR_DATE ( 2026, 8, 10 ) ;
#10713 = DIRECTION ( 'NONE',  ( -0.9997619372588931741, -0.000000000000000000, -0.02181900108494707821 ) ) ;
#10714 = ORIENTED_EDGE ( 'NONE', *, *, #10749, .F. ) ;
#10715 = ADVANCED_FACE ( 'NONE', ( #13057 ), #390, .F. ) ;
#10716 = VECTOR ( 'NONE', #14128, 1000.000000000000000 ) ;
#10717 = CARTESIAN_POINT ( 'NONE',  ( -12.27209645382210823, 2.500000000000000444, -127.2227734861304782 ) ) ;
#10718 = CARTESIAN_POINT ( 'NONE',  ( 3.749999999999998668, 12.18750000000000178, -5.053300858899108405 ) ) ;
#10719 = CARTESIAN_POINT ( 'NONE',  ( 4.351822957764132305, 0.03155975272378051116, -16.26963315870613869 ) ) ;
#10720 = CARTESIAN_POINT ( 'NONE',  ( -67.59870530518044518, 11.08167271862595094, -204.2373993420885370 ) ) ;
#10721 = CARTESIAN_POINT ( 'NONE',  ( 0.2625675448779695720, 5.000000000001672440, 2.974107436473219401 ) ) ;
#10722 = CARTESIAN_POINT ( 'NONE',  ( -1.346194077712558945, 1.562500000000000222, -0.2500000000000002220 ) ) ;
#10723 = VECTOR ( 'NONE', #1807, 1000.000000000000000 ) ;
#10724 = CARTESIAN_POINT ( 'NONE',  ( 8.807773658247754156, 15.00000000000000000, -105.8689255569352667 ) ) ;
#10725 = APPROVAL_DATE_TIME ( #10504, #13137 ) ;
#10726 = CARTESIAN_POINT ( 'NONE',  ( -4.706582913227679299, 13.87736884190558406, -125.1575984163914086 ) ) ;
#10727 = DIRECTION ( 'NONE',  ( -0.08794243244722420305, 0.000000000000000000, -0.9961255586397055328 ) ) ;
#10728 = ORIENTED_EDGE ( 'NONE', *, *, #12052, .T. ) ;
#10729 = EDGE_CURVE ( 'NONE', #13718, #5770, #13690, .T. ) ;
#10730 = CARTESIAN_POINT ( 'NONE',  ( 4.570349143970012129, 0.7032832823769218367, 2.199267984206088489 ) ) ;
#10731 = CARTESIAN_POINT ( 'NONE',  ( -1.346194077712558945, 3.062500000000000000, -0.2500000000000002220 ) ) ;
#10732 = EDGE_CURVE ( 'NONE', #5680, #1124, #5463, .T. ) ;
#10733 = CARTESIAN_POINT ( 'NONE',  ( -61.39244834783638538, 10.00000000000000000, -159.9779749835793723 ) ) ;
#10734 = CARTESIAN_POINT ( 'NONE',  ( 1.346194077712558279, 5.062500000000000000, -6.750000000000000888 ) ) ;
#10735 = ORIENTED_EDGE ( 'NONE', *, *, #12814, .F. ) ;
#10736 = CARTESIAN_POINT ( 'NONE',  ( -6.708306527933025620, 15.00000000000363798, -119.6038561067746855 ) ) ;
#10737 = CARTESIAN_POINT ( 'NONE',  ( -33.91109452335874153, 5.000000000000000000, -156.1716796081737471 ) ) ;
#10738 = CARTESIAN_POINT ( 'NONE',  ( 10.14988979988700457, 14.51423292646842889, -106.5995613745913602 ) ) ;
#10739 = CARTESIAN_POINT ( 'NONE',  ( -3.980102097228897245E-16, 2.500000000000000000, -6.749999999999999112 ) ) ;
#10740 = CARTESIAN_POINT ( 'NONE',  ( -4.592425496802573972E-16, 3.000000000000000444, -7.250000000000000000 ) ) ;
#10741 = CARTESIAN_POINT ( 'NONE',  ( 0.000000000000000000, 4.000000000000000000, 0.2500000000000002220 ) ) ;
#10742 = CARTESIAN_POINT ( 'NONE',  ( -35.49029739244799941, 5.000000000000000000, -131.2404697308744801 ) ) ;
#10743 = CARTESIAN_POINT ( 'NONE',  ( 3.749999999999999112, 6.187500000000001776, -5.053300858899108405 ) ) ;
#10744 = CARTESIAN_POINT ( 'NONE',  ( 4.021974294543523065, 14.95912548502000838, 0.5602530272244051757 ) ) ;
#10745 = CARTESIAN_POINT ( 'NONE',  ( -3.911881252916560747, 11.22597817734345860, -46.04150454295093908 ) ) ;
#10746 = CARTESIAN_POINT ( 'NONE',  ( -8.659520330960761569, 1.372957239594033263, -105.3656150850790141 ) ) ;
#10747 = DIRECTION ( 'NONE',  ( 0.000000000000000000, -1.000000000000000000, 0.000000000000000000 ) ) ;
#10748 = CARTESIAN_POINT ( 'NONE',  ( 3.249999999999999112, 12.81250000000000000, -2.153805922287439945 ) ) ;
#10749 = EDGE_CURVE ( 'NONE', #10866, #6397, #14439, .T. ) ;
#10750 = CARTESIAN_POINT ( 'NONE',  ( 6.023654006863524479, 0.4287155192450040064, 0.6418499716679767486 ) ) ;
#10751 = CARTESIAN_POINT ( 'NONE',  ( -65.17119078000779098, 14.57600458215128825, -195.0918058944346569 ) ) ;
#10752 = ORIENTED_EDGE ( 'NONE', *, *, #4243, .F. ) ;
#10753 = CARTESIAN_POINT ( 'NONE',  ( 3.749999999999999112, 9.187500000000001776, -5.053300858899108405 ) ) ;
#10754 = ORIENTED_EDGE ( 'NONE', *, *, #10368, .T. ) ;
#10755 = CARTESIAN_POINT ( 'NONE',  ( -6.790118584952986147, -1.321950343203052097E-12, -107.8021323225563179 ) ) ;
#10756 = CARTESIAN_POINT ( 'NONE',  ( -26.57518893882630096, 8.673617379884035472E-16, -201.5880480395080951 ) ) ;
#10757 = CARTESIAN_POINT ( 'NONE',  ( 2.651650429449553759, 4.875000000000000000, -0.8483495705504471296 ) ) ;
#10758 = CARTESIAN_POINT ( 'NONE',  ( 0.000000000000000000, 5.500000000000000000, 0.2499999999999998057 ) ) ;
#10759 = FACE_OUTER_BOUND ( 'NONE', #15150, .T. ) ;
#10760 = ORIENTED_EDGE ( 'NONE', *, *, #4309, .F. ) ;
#10761 = CARTESIAN_POINT ( 'NONE',  ( 1.346194077712561166, 6.437499999999999112, -0.2500000000000011102 ) ) ;
#10762 = CARTESIAN_POINT ( 'NONE',  ( -69.36122292260984068, 9.999999999999998224, -183.5207230678399810 ) ) ;
#10763 = B_SPLINE_CURVE_WITH_KNOTS ( 'NONE', 3,
 ( #1703, #6417, #554, #1472, #5266, #9976 ),
 .UNSPECIFIED., .F., .F.,
 ( 4, 2, 4 ),
 ( 0.000000000000000000, 0.006940540637791397204, 0.01388108127558279441 ),
 .UNSPECIFIED. ) ;
#10764 = CARTESIAN_POINT ( 'NONE',  ( 15.45423724370449214, 8.673617379884033500E-16, -134.7453193863913157 ) ) ;
#10765 = SHAPE_REPRESENTATION_RELATIONSHIP ( 'NONE' , 'NONE' ,  #4394, #7221 ) ;
#10766 = CARTESIAN_POINT ( 'NONE',  ( 3.249999999999999556, 6.750000000000000000, -3.500000000000000000 ) ) ;
#10767 = DIRECTION ( 'NONE',  ( 0.02058562339462769938, 0.3314513491899343522, -0.9432477061883729474 ) ) ;
#10768 = DIRECTION ( 'NONE',  ( 0.9939692226109180240, -0.000000000000000000, -0.1096594022519158940 ) ) ;
#10769 = CARTESIAN_POINT ( 'NONE',  ( 17.83675209366140280, 8.673617379884035472E-16, -136.7184283642698404 ) ) ;
#10770 = ORIENTED_EDGE ( 'NONE', *, *, #906, .T. ) ;
#10771 = DIRECTION ( 'NONE',  ( -0.000000000000000000, -1.000000000000000000, -0.000000000000000000 ) ) ;
#10772 = CARTESIAN_POINT ( 'NONE',  ( 1.243260443319662123, 6.000000000000000000, -139.4020581015306846 ) ) ;
#10773 = EDGE_LOOP ( 'NONE', ( #8400, #10434 ) ) ;
#10774 = ORIENTED_EDGE ( 'NONE', *, *, #14993, .T. ) ;
#10775 = DIRECTION ( 'NONE',  ( -0.000000000000000000, -1.000000000000000000, -0.000000000000000000 ) ) ;
#10776 = CARTESIAN_POINT ( 'NONE',  ( -3.750000000000000000, 6.812500000000001776, -5.053300858899105741 ) ) ;
#10777 = CARTESIAN_POINT ( 'NONE',  ( -3.980102097228897738E-16, 11.00000000000000000, -6.749999999999999112 ) ) ;
#10778 = VERTEX_POINT ( 'NONE', #4312 ) ;
#10779 = CARTESIAN_POINT ( 'NONE',  ( 10.22352057816269699, 15.00000000000000000, -125.5112093480189657 ) ) ;
#10780 = CARTESIAN_POINT ( 'NONE',  ( 3.249999999999998668, 5.687500000000000000, -4.846194077712560500 ) ) ;
#10781 = CARTESIAN_POINT ( 'NONE',  ( -7.091927898542184749, 0.03088880688819538659, -104.2116372605956656 ) ) ;
#10782 = CARTESIAN_POINT ( 'NONE',  ( -37.06343578980261810, 10.00000000000000355, -156.4760336361639474 ) ) ;
#10783 = CARTESIAN_POINT ( 'NONE',  ( -41.68741913287574619, 15.00000000000000178, -152.6276280980627291 ) ) ;
#10784 = APPROVAL_ROLE ( '' ) ;
#10785 = CARTESIAN_POINT ( 'NONE',  ( -19.94423925787078389, 15.00000000000000000, -150.2885610952392881 ) ) ;
#10786 = CLOSED_SHELL ( 'NONE', ( #8534, #14058, #11945, #11875, #7905, #4117, #13115, #918, #11604, #12335, #3014, #11269, #2429, #14748, #5906, #5126, #1924 ) ) ;
#10787 = ORIENTED_EDGE ( 'NONE', *, *, #7323, .T. ) ;
#10788 = CARTESIAN_POINT ( 'NONE',  ( 3.249999999999998224, 14.31250000000000355, -2.153805922287439945 ) ) ;
#10789 = CARTESIAN_POINT ( 'NONE',  ( 2.850044070969222076, 5.000000000000000888, -103.0233998225063345 ) ) ;
#10791 = CARTESIAN_POINT ( 'NONE',  ( 3.749999999999999556, 12.25000000000000000, -3.500000000000000444 ) ) ;
#10790 = SHAPE_REPRESENTATION ( 'Washer_Predeterminado', ( #9419 ), #2511 ) ;
#10792 = EDGE_CURVE ( 'NONE', #447, #1413, #7752, .T. ) ;
#10793 = CARTESIAN_POINT ( 'NONE',  ( -67.58382171872797528, 10.11977001915115437, -204.5178482232321642 ) ) ;
#10794 = CARTESIAN_POINT ( 'NONE',  ( 29.21736815051483660, 8.773889247172311556, -44.21329492081407153 ) ) ;
#10795 = CARTESIAN_POINT ( 'NONE',  ( -3.980102097228897738E-16, 2.000000000000000000, -6.749999999999999112 ) ) ;
#10796 = CARTESIAN_POINT ( 'NONE',  ( 9.673258414158063090, 1.297355693541400345, -105.9236831072048375 ) ) ;
#10797 = PERSON_AND_ORGANIZATION_ROLE ( 'creator' ) ;
#10798 = CARTESIAN_POINT ( 'NONE',  ( 9.044950117654433797, -4.000000000000000000, -141.4826476090360643 ) ) ;
#10799 = CARTESIAN_POINT ( 'NONE',  ( -17.32624372124044854, 0.6199615622964459449, -130.2318118670719116 ) ) ;
#10800 = EDGE_LOOP ( 'NONE', ( #6867, #10506, #13865, #1271 ) ) ;
#10801 = CARTESIAN_POINT ( 'NONE',  ( 5.602568457641995181, 0.2629148106111021677, 0.1074933644148804157 ) ) ;
#10802 = CARTESIAN_POINT ( 'NONE',  ( -3.249999999999999556, 5.312500000000000888, -4.846194077712557835 ) ) ;
#10803 = CYLINDRICAL_SURFACE ( 'NONE', #8391, 1.000000000000000888 ) ;
#10804 = CARTESIAN_POINT ( 'NONE',  ( -1.346194077712559167, 0.9375000000000000000, -6.749999999999999112 ) ) ;
#10805 = CARTESIAN_POINT ( 'NONE',  ( 1.346194077712558279, 7.062500000000000888, -6.750000000000000888 ) ) ;
#10806 = CARTESIAN_POINT ( 'NONE',  ( -8.431010172718810480, 15.00000000000000000, -122.5582262044626844 ) ) ;
#10807 = CARTESIAN_POINT ( 'NONE',  ( -0.1255007366002022229, -0.2049726491322196309, -0.1347136637248375068 ) ) ;
#10808 = CARTESIAN_POINT ( 'NONE',  ( -7.136800800249558208, 9.999999999999998224, -146.1984219327868288 ) ) ;
#10809 = CARTESIAN_POINT ( 'NONE',  ( -3.980102097228897245E-16, 1.500000000000000000, -6.749999999999999112 ) ) ;
#10810 = CARTESIAN_POINT ( 'NONE',  ( -1.553300858899106629, 2.562500000000000444, 0.2499999999999998335 ) ) ;
#10811 = CARTESIAN_POINT ( 'NONE',  ( -3.750000000000000000, 4.250000000000000000, -3.499999999999999112 ) ) ;
#10812 = CARTESIAN_POINT ( 'NONE',  ( -3.395812927963546723, 10.62992796920838678, -45.78929837901311117 ) ) ;
#10813 = CARTESIAN_POINT ( 'NONE',  ( 3.749999999999999112, 5.187500000000001776, -5.053300858899108405 ) ) ;
#10814 = CARTESIAN_POINT ( 'NONE',  ( 0.6968013826459904525, 11.59070670907840928, 5.520114370516503222 ) ) ;
#10815 = EDGE_CURVE ( 'NONE', #11706, #11348, #13740, .T. ) ;
#10816 = CARTESIAN_POINT ( 'NONE',  ( -12.27209645382210823, 15.00000000000000000, -127.2227734861304782 ) ) ;
#10817 = CARTESIAN_POINT ( 'NONE',  ( 13.13192191588670887, 4.000000000000000000, -166.1703390355876877 ) ) ;
#10818 = DIRECTION ( 'NONE',  ( 0.000000000000000000, 1.000000000000000000, 0.000000000000000000 ) ) ;
#10819 = LINE ( 'NONE', #4036, #14352 ) ;
#10820 = CARTESIAN_POINT ( 'NONE',  ( -12.30607691012835403, 8.673617379884034486E-16, -158.4081044807556111 ) ) ;
#10821 = CARTESIAN_POINT ( 'NONE',  ( -65.22313063405162836, 14.79918553424455041, -191.8929365503416022 ) ) ;
#10822 = CARTESIAN_POINT ( 'NONE',  ( 2.298097038856279362, 8.875000000000001776, -1.201902961143720860 ) ) ;
#10823 = ORIENTED_EDGE ( 'NONE', *, *, #6476, .T. ) ;
#10824 = CARTESIAN_POINT ( 'NONE',  ( -3.750000000000000000, 9.812500000000000000, -5.053300858899105741 ) ) ;
#10825 = ORIENTED_EDGE ( 'NONE', *, *, #12216, .T. ) ;
#10826 = CARTESIAN_POINT ( 'NONE',  ( -7.473411123415157675, 4.336808689942017736E-16, -120.9918979908683525 ) ) ;
#10827 = CARTESIAN_POINT ( 'NONE',  ( -7.194037649453649763, -1.020558061026470176, -45.55632290616381397 ) ) ;
#10828 = CARTESIAN_POINT ( 'NONE',  ( -3.750000000000000000, 9.250000000000000000, -3.499999999999999112 ) ) ;
#10829 = CARTESIAN_POINT ( 'NONE',  ( -4.592425496802573972E-16, 5.000000000000000000, -7.250000000000000000 ) ) ;
#10830 = LINE ( 'NONE', #7275, #10694 ) ;
#10831 = EDGE_LOOP ( 'NONE', ( #3823, #727, #13866, #9854 ) ) ;
#10832 = CARTESIAN_POINT ( 'NONE',  ( 1.346194077712558279, 3.062500000000000000, -6.750000000000000888 ) ) ;
#10833 = ADVANCED_FACE ( 'NONE', ( #4022 ), #6333, .F. ) ;
#10834 = CARTESIAN_POINT ( 'NONE',  ( 3.750000000000000000, 9.750000000000000000, -3.500000000000000444 ) ) ;
#10835 = CARTESIAN_POINT ( 'NONE',  ( -64.93158582249934341, 15.00000000000000000, -188.2511415724482049 ) ) ;
#10836 = EDGE_CURVE ( 'NONE', #13395, #14298, #11412, .T. ) ;
#10837 = ADVANCED_FACE ( 'NONE', ( #2784 ), #1621, .T. ) ;
#10838 = CARTESIAN_POINT ( 'NONE',  ( -1.528156170053301510, 7.379999999999995453, -45.73714083922575213 ) ) ;
#10839 = CARTESIAN_POINT ( 'NONE',  ( 1.346194077712558057, 7.562500000000000000, -6.750000000000000000 ) ) ;
#10840 = CARTESIAN_POINT ( 'NONE',  ( 5.844703153020811115, 0.000000000000000000, -103.2023327213425432 ) ) ;
#10841 =( REPRESENTATION_RELATIONSHIP ('NONE','NONE', #11394, #9812 ) REPRESENTATION_RELATIONSHIP_WITH_TRANSFORMATION ( #6829 )SHAPE_REPRESENTATION_RELATIONSHIP( ) );
#10842 = APPROVAL_STATUS ( 'not_yet_approved' ) ;
#10843 = CARTESIAN_POINT ( 'NONE',  ( 4.286263797015736595E-16, 5.000000000000000000, 3.500000000000000000 ) ) ;
#10844 = CARTESIAN_POINT ( 'NONE',  ( 10.46664703690589349, 5.000000000000000888, -121.2724779346276875 ) ) ;
#10845 = ORIENTED_EDGE ( 'NONE', *, *, #9246, .T. ) ;
#10846 = PLANE ( 'NONE',  #1747 ) ;
#10847 = CARTESIAN_POINT ( 'NONE',  ( -8.765409998386077817, -2.075239479414269894, -35.06535713112702979 ) ) ;
#10848 = ORIENTED_EDGE ( 'NONE', *, *, #4845, .T. ) ;
#10849 = EDGE_LOOP ( 'NONE', ( #1834, #13024, #2415, #1434 ) ) ;
#10850 = LINE ( 'NONE', #501, #5279 ) ;
#10851 = CARTESIAN_POINT ( 'NONE',  ( 2.651650429449552870, 12.12500000000000000, -6.151650429449553314 ) ) ;
#10852 = CARTESIAN_POINT ( 'NONE',  ( -2.298097038856278029, 6.625000000000000000, -1.201902961143720638 ) ) ;
#10853 = CARTESIAN_POINT ( 'NONE',  ( 3.249999999999999556, 10.25000000000000178, -3.500000000000000000 ) ) ;
#10854 = ORIENTED_EDGE ( 'NONE', *, *, #11504, .F. ) ;
#10855 = CARTESIAN_POINT ( 'NONE',  ( 1.052436484934202499, -2.075239479414269894, -1.000000000000000888 ) ) ;
#10856 = CARTESIAN_POINT ( 'NONE',  ( -3.249999999999999556, 7.187500000000000000, -2.153805922287440833 ) ) ;
#10857 = CC_DESIGN_APPROVAL ( #4690, ( #10116 ) ) ;
#10858 = AXIS2_PLACEMENT_3D ( 'NONE', #11547, #3202, #15129 ) ;
#10859 = CARTESIAN_POINT ( 'NONE',  ( -6.790153584124027475, 9.999999999999998224, -124.9643354754709748 ) ) ;
#10860 = CARTESIAN_POINT ( 'NONE',  ( -43.45809816649217083, 10.00000000000000000, -159.1057901742589422 ) ) ;
#10861 = DIRECTION ( 'NONE',  ( 0.000000000000000000, 0.000000000000000000, 1.000000000000000000 ) ) ;
#10862 = PERSON_AND_ORGANIZATION_ROLE ( 'design_owner' ) ;
#10863 = APPROVAL ( #65, 'UNSPECIFIED' ) ;
#10864 = LINE ( 'NONE', #9713, #2582 ) ;
#10865 = SECURITY_CLASSIFICATION ( '', '', #11996 ) ;
#10866 = VERTEX_POINT ( 'NONE', #2063 ) ;
#10867 = CARTESIAN_POINT ( 'NONE',  ( -3.249999999999999556, 2.312500000000000888, -4.846194077712557835 ) ) ;
#10868 = CARTESIAN_POINT ( 'NONE',  ( -1.553300858899107295, 14.43750000000000000, -7.250000000000000000 ) ) ;
#10869 = AXIS2_PLACEMENT_3D ( 'NONE', #9371, #1341, #13085 ) ;
#10870 = CARTESIAN_POINT ( 'NONE',  ( 13.78275167297412906, 13.34157715675068623, -126.2206732457524794 ) ) ;
#10871 = CARTESIAN_POINT ( 'NONE',  ( -2.651650429449552870, 12.87500000000000178, -6.151650429449552426 ) ) ;
#10872 = TOROIDAL_SURFACE ( 'NONE', #13363, 3.750000000000003553, 0.5000000000000000000 ) ;
#10873 = CARTESIAN_POINT ( 'NONE',  ( -63.93680978957204530, 12.84083462876305859, -201.7870368253884692 ) ) ;
#10874 = LINE ( 'NONE', #3928, #11393 ) ;
#10875 = CARTESIAN_POINT ( 'NONE',  ( -2.298097038856278029, 3.625000000000000888, -1.201902961143720638 ) ) ;
#10876 = CARTESIAN_POINT ( 'NONE',  ( 6.288457687478774538, 8.673617379884035472E-16, -105.0111312234652985 ) ) ;
#10877 = AXIS2_PLACEMENT_3D ( 'NONE', #8808, #13465, #3153 ) ;
#10878 = COORDINATED_UNIVERSAL_TIME_OFFSET ( 0, 0, .AHEAD. ) ;
#10879 = CARTESIAN_POINT ( 'NONE',  ( -4.924771681124648026, 0.000000000000000000, -137.0932397189673111 ) ) ;
#10880 = CARTESIAN_POINT ( 'NONE',  ( 1.123679064339592859, 4.590773665857039276, -139.4222662838609210 ) ) ;
#10881 = ORIENTED_EDGE ( 'NONE', *, *, #12073, .T. ) ;
#10882 = CARTESIAN_POINT ( 'NONE',  ( 6.533497844638413987, 0.7032832832067333895, 1.143078642481199614 ) ) ;
#10883 = CARTESIAN_POINT ( 'NONE',  ( -2.298097038856278918, 6.375000000000000888, -5.798097038856277585 ) ) ;
#10884 = EDGE_CURVE ( 'NONE', #14114, #3665, #14937, .T. ) ;
#10885 = EDGE_CURVE ( 'NONE', #750, #1255, #12205, .T. ) ;
#10886 = FACE_OUTER_BOUND ( 'NONE', #5410, .T. ) ;
#10887 = CARTESIAN_POINT ( 'NONE',  ( 3.249999999999998224, 1.187499999999999778, -4.846194077712561388 ) ) ;
#10888 = VECTOR ( 'NONE', #8701, 1000.000000000000114 ) ;
#10889 = CARTESIAN_POINT ( 'NONE',  ( 3.249999999999998224, 11.18750000000000178, -4.846194077712561388 ) ) ;
#10890 = CARTESIAN_POINT ( 'NONE',  ( -0.7473297648211070232, 15.00000000000000000, -117.8744674975950488 ) ) ;
#10891 = SHAPE_REPRESENTATION ( 'Blade_Predeterminado', ( #9419 ), #12893 ) ;
#10892 = CARTESIAN_POINT ( 'NONE',  ( 1.034717776212374707, 12.74535153223338035, 2.425209233265293918 ) ) ;
#10893 = CARTESIAN_POINT ( 'NONE',  ( 9.379784756826319736, 14.94013921591925076, -106.1734080947524319 ) ) ;
#10894 = CARTESIAN_POINT ( 'NONE',  ( -3.249999999999999556, 6.312500000000000888, -4.846194077712557835 ) ) ;
#10895 = CARTESIAN_POINT ( 'NONE',  ( 2.298097038856279362, 15.37500000000000178, -1.201902961143720860 ) ) ;
#10896 = CARTESIAN_POINT ( 'NONE',  ( 3.749999999999999556, 5.812500000000000000, -1.946699141100892261 ) ) ;
#10897 = CARTESIAN_POINT ( 'NONE',  ( 0.06918667591891866642, 2.515825626418123573, 0.7836787576023231949 ) ) ;
#10898 = CARTESIAN_POINT ( 'NONE',  ( 2.651650429449552870, 5.125000000000000888, -6.151650429449555091 ) ) ;
#10899 = CARTESIAN_POINT ( 'NONE',  ( 1.242364750776129290, 13.05645226862330333, 2.267205653757014439 ) ) ;
#10900 = CARTESIAN_POINT ( 'NONE',  ( 11.77584962622735887, 1.499941477809432211, -165.6889925597199351 ) ) ;
#10901 = CARTESIAN_POINT ( 'NONE',  ( -8.871974675278494260, 2.162842538941835979, -105.5068606680567882 ) ) ;
#10902 = DIRECTION ( 'NONE',  ( 0.000000000000000000, 0.000000000000000000, -1.000000000000000000 ) ) ;
#10903 = CARTESIAN_POINT ( 'NONE',  ( -0.3766621274091715987, 0.2613176957160640579, -6.863050255469941519 ) ) ;
#10904 = CARTESIAN_POINT ( 'NONE',  ( 4.999884422966211162, 0.09518442032929252949, -1.466239102699074870 ) ) ;
#10905 = CARTESIAN_POINT ( 'NONE',  ( 3.136841903360914952, -5.204170427930421283E-15, -104.4936450199714812 ) ) ;
#10906 = EDGE_LOOP ( 'NONE', ( #7523, #427, #9197, #1218 ) ) ;
#10907 = EDGE_CURVE ( 'NONE', #11355, #6678, #7126, .T. ) ;
#10908 = CARTESIAN_POINT ( 'NONE',  ( -2.651650429449553314, 8.874999999999996447, -6.151650429449552426 ) ) ;
#10909 = EDGE_LOOP ( 'NONE', ( #13073, #4652, #15086, #1511 ) ) ;
#10910 = CARTESIAN_POINT ( 'NONE',  ( -4.234261469891104745, 4.336808689942017736E-16, -107.1714994797973475 ) ) ;
#10911 = CARTESIAN_POINT ( 'NONE',  ( -16.79479163992151669, 8.673617379884035472E-16, -186.8953034624466909 ) ) ;
#10912 = CARTESIAN_POINT ( 'NONE',  ( 1.553300858899105963, 9.562500000000000000, -7.250000000000000888 ) ) ;
#10913 = CARTESIAN_POINT ( 'NONE',  ( 1.553300858899109071, 8.437500000000000000, 0.2499999999999989175 ) ) ;
#10914 = DIRECTION ( 'NONE',  ( 1.000000000000000000, 0.000000000000000000, 0.000000000000000000 ) ) ;
#10915 = ORIENTED_EDGE ( 'NONE', *, *, #9195, .F. ) ;
#10916 = LOCAL_TIME ( 12, 28, 20.00000000000000000, #2456 ) ;
#10917 = CARTESIAN_POINT ( 'NONE',  ( -7.687033461059511019, 1.096071398028247046, -116.8257989789358220 ) ) ;
#10918 = CARTESIAN_POINT ( 'NONE',  ( -3.980102097228897738E-16, 5.000000000000000000, -6.749999999999999112 ) ) ;
#10919 = CARTESIAN_POINT ( 'NONE',  ( -2.651650429449553314, 10.37500000000000000, -6.151650429449552426 ) ) ;
#10920 = CARTESIAN_POINT ( 'NONE',  ( -70.09987374443890928, 9.999999999999998224, -191.4540390840369355 ) ) ;
#10921 = DIRECTION ( 'NONE',  ( 0.1564344650402314796, 0.000000000000000000, 0.9876883405951375483 ) ) ;
#10922 = DIRECTION ( 'NONE',  ( -0.003262051938530596308, 0.000000000000000000, 0.9999946794944214457 ) ) ;
#10923 = CARTESIAN_POINT ( 'NONE',  ( 3.249999999999998668, 6.687500000000000888, -4.846194077712560500 ) ) ;
#10924 = CARTESIAN_POINT ( 'NONE',  ( -2.722152201699274521, 7.379999999999995453, -47.89048091371786597 ) ) ;
#10925 = DATE_AND_TIME ( #13255, #256 ) ;
#10926 = CARTESIAN_POINT ( 'NONE',  ( -6.027592497978528918, 4.999999999999210409, -126.6584150166564768 ) ) ;
#10927 = DIRECTION ( 'NONE',  ( -0.000000000000000000, -1.000000000000000000, -0.000000000000000000 ) ) ;
#10928 = ORIENTED_EDGE ( 'NONE', *, *, #12623, .F. ) ;
#10929 = LINE ( 'NONE', #6440, #13103 ) ;
#10930 = CARTESIAN_POINT ( 'NONE',  ( -1.346194077712558945, 13.06250000000000000, -0.2500000000000002220 ) ) ;
#10931 = ORIENTED_EDGE ( 'NONE', *, *, #12531, .F. ) ;
#10932 = ADVANCED_FACE ( 'NONE', ( #6624 ), #6558, .F. ) ;
#10933 = ORIENTED_EDGE ( 'NONE', *, *, #13517, .T. ) ;
#10934 = DIRECTION ( 'NONE',  ( 0.000000000000000000, 0.000000000000000000, 1.000000000000000000 ) ) ;
#10935 = CARTESIAN_POINT ( 'NONE',  ( 3.749999999999998668, 12.18750000000000178, -5.053300858899108405 ) ) ;
#10936 = CARTESIAN_POINT ( 'NONE',  ( -3.249999999999999112, 12.81250000000000178, -4.846194077712558723 ) ) ;
#10937 = EDGE_CURVE ( 'NONE', #1534, #5560, #4100, .T. ) ;
#10938 = CARTESIAN_POINT ( 'NONE',  ( 3.249999999999999556, 11.25000000000000000, -3.500000000000000000 ) ) ;
#10940 = EDGE_CURVE ( 'NONE', #882, #12098, #3486, .T. ) ;
#10939 = ORIENTED_EDGE ( 'NONE', *, *, #2304, .T. ) ;
#10941 = CARTESIAN_POINT ( 'NONE',  ( -8.199037228204968386, 15.00000000003875478, -114.3845095685942255 ) ) ;
#10942 = CARTESIAN_POINT ( 'NONE',  ( -1.346194077712559389, 5.437500000000002665, -6.749999999999999112 ) ) ;
#10943 = CARTESIAN_POINT ( 'NONE',  ( -9.721966606378851239, 10.00000000000000000, -116.3614657639809309 ) ) ;
#10944 = CARTESIAN_POINT ( 'NONE',  ( 4.025564746441875563, 0.09586553063150847487, -1.251268110428811697 ) ) ;
#10945 = CARTESIAN_POINT ( 'NONE',  ( -4.507463604512252253, 0.000000000000000000, -2.585105772303598393 ) ) ;
#10946 = TOROIDAL_SURFACE ( 'NONE', #9948, 9.499999999999941380, 2.500000000000000000 ) ;
#10947 = DATE_TIME_ROLE ( 'classification_date' ) ;
#10948 = CARTESIAN_POINT ( 'NONE',  ( -24.61436772009224327, 4.000000000000000000, -208.9121151917288728 ) ) ;
#10949 = ORIENTED_EDGE ( 'NONE', *, *, #1446, .F. ) ;
#10950 = CARTESIAN_POINT ( 'NONE',  ( 3.249999999999999556, 9.750000000000000000, -3.500000000000000000 ) ) ;
#10951 = CARTESIAN_POINT ( 'NONE',  ( 1.346194077712558057, 2.562500000000000444, -6.750000000000000000 ) ) ;
#10952 = CARTESIAN_POINT ( 'NONE',  ( 3.750000000000000000, 14.75000000000000178, -3.500000000000000444 ) ) ;
#10953 = ADVANCED_FACE ( 'NONE', ( #9644 ), #11800, .F. ) ;
#10954 = DIRECTION ( 'NONE',  ( 0.000000000000000000, -1.000000000000000000, 0.000000000000000000 ) ) ;
#10955 = AXIS2_PLACEMENT_3D ( 'NONE', #8974, #1513, #6224 ) ;
#10956 = CIRCLE ( 'NONE', #14926, 16.00000000006737721 ) ;
#10957 = CARTESIAN_POINT ( 'NONE',  ( -1.553300858899106629, 0.06250000000000002776, 0.2500000000000002220 ) ) ;
#10958 = CARTESIAN_POINT ( 'NONE',  ( -63.77135710064911223, 12.50589072853210482, -202.2543161940598679 ) ) ;
#10959 = DIRECTION ( 'NONE',  ( 0.02181900108494737658, 0.000000000000000000, -0.9997619372588931741 ) ) ;
#10960 = CARTESIAN_POINT ( 'NONE',  ( 6.605878363002800846, 8.242932226922413110E-11, -105.1138548165823607 ) ) ;
#10961 = PERSON_AND_ORGANIZATION ( #3176, #3020 ) ;
#10962 = CARTESIAN_POINT ( 'NONE',  ( -66.93602132738925548, 14.64151217242501701, -194.2073690153594612 ) ) ;
#10963 = CIRCLE ( 'NONE', #14684, 3.000000000000010214 ) ;
#10964 = CARTESIAN_POINT ( 'NONE',  ( 0.01496453197139708223, 5.000000000000000000, 5.196130874293197088 ) ) ;
#10965 = ORIENTED_EDGE ( 'NONE', *, *, #2054, .F. ) ;
#10966 = CARTESIAN_POINT ( 'NONE',  ( 4.999884244121599153, 0.09548446344527571072, -1.396462267504845922 ) ) ;
#10967 = CARTESIAN_POINT ( 'NONE',  ( 1.346194077712560944, 6.937500000000000000, -0.2500000000000011102 ) ) ;
#10968 = CARTESIAN_POINT ( 'NONE',  ( -70.05680446119299631, 10.00000000000000178, -194.6833061307580977 ) ) ;
#10969 = CARTESIAN_POINT ( 'NONE',  ( 1.346194077712560944, 11.93750000000000000, -0.2500000000000010547 ) ) ;
#10970 = CARTESIAN_POINT ( 'NONE',  ( -3.980102097228897738E-16, 12.00000000000000178, -6.749999999999999112 ) ) ;
#10971 = DIRECTION ( 'NONE',  ( 0.1096594022519158801, 0.000000000000000000, 0.9939692226109179130 ) ) ;
#10972 = CARTESIAN_POINT ( 'NONE',  ( -3.249999999999999556, 0.2500000000000000000, -3.499999999999999556 ) ) ;
#10973 = CARTESIAN_POINT ( 'NONE',  ( 10.77692171413472977, 14.06121913176011162, -106.2890056980015743 ) ) ;
#10974 = CARTESIAN_POINT ( 'NONE',  ( -2.298097038856278918, 4.375000000000000000, -5.798097038856277585 ) ) ;
#10975 = AXIS2_PLACEMENT_3D ( 'NONE', #14277, #1286, #5989 ) ;
#10976 = CARTESIAN_POINT ( 'NONE',  ( -3.249999999999999112, 14.68750000000000178, -2.153805922287440833 ) ) ;
#10977 = CARTESIAN_POINT ( 'NONE',  ( -1.553300858899106407, 4.062500000000000000, 0.2500000000000002220 ) ) ;
#10978 = CARTESIAN_POINT ( 'NONE',  ( -3.331923142838100205, 10.52305467079069778, -44.71953693998822388 ) ) ;
#10979 = CARTESIAN_POINT ( 'NONE',  ( 3.749999999999999112, 7.187500000000000888, -5.053300858899108405 ) ) ;
#10980 = CARTESIAN_POINT ( 'NONE',  ( 0.7636165113260954262, 12.24296972256808402, 2.624416505665311927 ) ) ;
#10981 = CARTESIAN_POINT ( 'NONE',  ( 11.93152510496921792, 1.468982674681399425, -165.5488479599881657 ) ) ;
#10982 = CARTESIAN_POINT ( 'NONE',  ( 21.72409770179331545, 4.000000000000000000, -147.6411415183954432 ) ) ;
#10983 = CARTESIAN_POINT ( 'NONE',  ( -8.141143895042660006, 3.999999999999993783, -146.5791559415450536 ) ) ;
#10984 = CARTESIAN_POINT ( 'NONE',  ( 5.538592533983068833, 2.409808734938486930E-16, -141.6430817385786725 ) ) ;
#10985 =( BOUNDED_SURFACE ( )  B_SPLINE_SURFACE ( 3, 2, ( 
 ( #12948, #11921, #1347 ),
 ( #13092, #10542, #5890 ),
 ( #9692, #6050, #7118 ),
 ( #263, #13020, #1119 ),
 ( #2507, #185, #10769 ),
 ( #15276, #14423, #11841 ),
 ( #13176, #4896, #7285 ),
 ( #110, #6984, #9377 ),
 ( #8445, #5971, #7203 ),
 ( #2279, #4824, #14337 ),
 ( #10612, #34, #1424 ),
 ( #3739, #10692, #11998 ),
 ( #6129, #12867, #9536 ),
 ( #10844, #4974, #3822 ),
 ( #14262, #11701, #9460 ),
 ( #3661, #8362, #5820 ),
 ( #14108, #3510, #8216 ),
 ( #2355, #11769, #1187 ),
 ( #14186, #3591, #8292 ),
 ( #11008, #1723, #11077 ),
 ( #5288, #6518, #14809 ),
 ( #1652, #8523, #495 ),
 ( #2742, #654, #13417 ),
 ( #4060, #14502, #3979 ),
 ( #1577, #5213, #2662 ),
 ( #7445, #8683, #344 ),
 ( #8835, #7594, #422 ),
 ( #13257, #6365, #5132 ),
 ( #2820, #11156, #10073 ),
 ( #14735, #13562, #4134 ),
 ( #9924, #2962, #6439 ),
 ( #14657, #5358, #12162 ),
 ( #8764, #7363, #7674 ),
 ( #13494, #10000, #8599 ),
 ( #12077, #2893, #12309 ),
 ( #576, #7522, #12387 ) ),
 .UNSPECIFIED., .F., .F., .F. ) 
 B_SPLINE_SURFACE_WITH_KNOTS ( ( 4, 2, 2, 2, 2, 2, 2, 2, 2, 2, 2, 2, 2, 2, 2, 2, 2, 4 ),
 ( 3, 3 ),
 ( 0.04342216404570826971, 0.04926220847718112278, 0.05218223069291755278, 0.05510225290865397585, 0.06094229734012682892, 0.06678234177159968199, 0.06824235287946789352, 0.06970236398733611893, 0.07262238620307254200, 0.07554240841880896506, 0.07700241952667717660, 0.07846243063454538813, 0.08138245285028181120, 0.08284246395815002273, 0.08430247506601823426, 0.08576248617388644579, 0.08722249728175465733, 0.09014251949749109427 ),
 ( 0.000000000000000000, 1.000000000000000000 ),
 .UNSPECIFIED. ) 
 GEOMETRIC_REPRESENTATION_ITEM ( )  RATIONAL_B_SPLINE_SURFACE ( (
 ( 1.000000000000000000, 0.7071067811865475727, 1.000000000000000000),
 ( 1.000000000000000000, 0.7071067811865475727, 1.000000000000000000),
 ( 1.000000000000000000, 0.7071067811865475727, 1.000000000000000000),
 ( 1.000000000000000000, 0.7071067811865475727, 1.000000000000000000),
 ( 1.000000000000000000, 0.7071067811865475727, 1.000000000000000000),
 ( 1.000000000000000000, 0.7071067811865475727, 1.000000000000000000),
 ( 1.000000000000000000, 0.7071067811865475727, 1.000000000000000000),
 ( 1.000000000000000000, 0.7071067811865475727, 1.000000000000000000),
 ( 1.000000000000000000, 0.7071067811865474617, 1.000000000000000000),
 ( 1.000000000000000000, 0.7071067811865474617, 1.000000000000000000),
 ( 1.000000000000000000, 0.7071067811865475727, 1.000000000000000000),
 ( 1.000000000000000000, 0.7071067811865475727, 1.000000000000000000),
 ( 1.000000000000000000, 0.7071067811865475727, 1.000000000000000000),
 ( 1.000000000000000000, 0.7071067811865475727, 1.000000000000000000),
 ( 1.000000000000000000, 0.7071067811865475727, 1.000000000000000000),
 ( 1.000000000000000000, 0.7071067811865475727, 1.000000000000000000),
 ( 1.000000000000000000, 0.7071067811865475727, 1.000000000000000000),
 ( 1.000000000000000000, 0.7071067811865475727, 1.000000000000000000),
 ( 1.000000000000000000, 0.7071067811865474617, 1.000000000000000000),
 ( 1.000000000000000000, 0.7071067811865474617, 1.000000000000000000),
 ( 1.000000000000000000, 0.7071067811865474617, 1.000000000000000000),
 ( 1.000000000000000000, 0.7071067811865474617, 1.000000000000000000),
 ( 1.000000000000000000, 0.7071067811865474617, 1.000000000000000000),
 ( 1.000000000000000000, 0.7071067811865474617, 1.000000000000000000),
 ( 1.000000000000000000, 0.7071067811865475727, 1.000000000000000000),
 ( 1.000000000000000000, 0.7071067811865475727, 1.000000000000000000),
 ( 1.000000000000000000, 0.7071067811865475727, 1.000000000000000000),
 ( 1.000000000000000000, 0.7071067811865475727, 1.000000000000000000),
 ( 1.000000000000000000, 0.7071067811865475727, 1.000000000000000000),
 ( 1.000000000000000000, 0.7071067811865475727, 1.000000000000000000),
 ( 1.000000000000000000, 0.7071067811865475727, 1.000000000000000000),
 ( 1.000000000000000000, 0.7071067811865475727, 1.000000000000000000),
 ( 1.000000000000000000, 0.7071067811865475727, 1.000000000000000000),
 ( 1.000000000000000000, 0.7071067811865475727, 1.000000000000000000),
 ( 1.000000000000000000, 0.7071067811865482389, 1.000000000000000000),
 ( 1.000000000000000000, 0.7071067811865482389, 1.000000000000000000) ) ) 
 REPRESENTATION_ITEM ( '' )  SURFACE ( )  );
#10986 = CARTESIAN_POINT ( 'NONE',  ( 5.101173563692228186, 0.1187549523756990522, -0.9191412569148569300 ) ) ;
#10987 = ORIENTED_EDGE ( 'NONE', *, *, #3565, .F. ) ;
#10988 = CARTESIAN_POINT ( 'NONE',  ( -3.249999999999999112, -0.1874999999999998890, -4.846194077712558723 ) ) ;
#10989 = VERTEX_POINT ( 'NONE', #2615 ) ;
#10990 = FACE_OUTER_BOUND ( 'NONE', #2508, .T. ) ;
#10991 = CARTESIAN_POINT ( 'NONE',  ( 5.376486659670671742, -1.020558061026470176, -45.55632290616389923 ) ) ;
#10992 = CARTESIAN_POINT ( 'NONE',  ( 3.749999999999998668, 10.68750000000000000, -5.053300858899107517 ) ) ;
#10993 = CARTESIAN_POINT ( 'NONE',  ( 2.651650429449552870, 7.124999999999999112, -6.151650429449553314 ) ) ;
#10994 = LINE ( 'NONE', #13165, #14425 ) ;
#10995 = ORIENTED_EDGE ( 'NONE', *, *, #6671, .T. ) ;
#10996 = CARTESIAN_POINT ( 'NONE',  ( 1.346194077712558279, 4.062500000000001776, -6.750000000000000888 ) ) ;
#10997 = ADVANCED_FACE ( 'NONE', ( #1215 ), #14978, .F. ) ;
#10998 = EDGE_CURVE ( 'NONE', #114, #11706, #8398, .T. ) ;
#10999 = CARTESIAN_POINT ( 'NONE',  ( 1.553300858899108849, 9.937499999999998224, 0.2499999999999993616 ) ) ;
#11000 = CARTESIAN_POINT ( 'NONE',  ( -65.10629832468505640, 15.00000000000000000, -192.2002039375829554 ) ) ;
#11001 = LINE ( 'NONE', #14497, #5199 ) ;
#11002 = EDGE_CURVE ( 'NONE', #14278, #8296, #13326, .T. ) ;
#11003 = APPLICATION_PROTOCOL_DEFINITION ( 'international standard', 'config_control_design', 1994, #8779 ) ;
#11004 = CARTESIAN_POINT ( 'NONE',  ( -1.346194077712559389, 7.062500000000000000, -0.2500000000000002220 ) ) ;
#11005 = LINE ( 'NONE', #13173, #10054 ) ;
#11006 = DATE_AND_TIME ( #261, #14083 ) ;
#11007 = CARTESIAN_POINT ( 'NONE',  ( -9.247150027671290573, -2.758321981116462875E-12, -118.2023151953508773 ) ) ;
#11008 = CARTESIAN_POINT ( 'NONE',  ( 8.481465556139287543, 5.000000000000000888, -115.9036014638648453 ) ) ;
#11009 = ORIENTED_EDGE ( 'NONE', *, *, #8440, .F. ) ;
#11010 = CARTESIAN_POINT ( 'NONE',  ( 4.999999999999997335, 0.000000000000000000, -108.9020125831789727 ) ) ;
#11011 = FACE_OUTER_BOUND ( 'NONE', #14992, .T. ) ;
#11012 = ORIENTED_EDGE ( 'NONE', *, *, #7385, .T. ) ;
#11013 = ORIENTED_EDGE ( 'NONE', *, *, #2622, .F. ) ;
#11014 = CARTESIAN_POINT ( 'NONE',  ( 2.159942170319879562, 15.00000000000000000, -121.5147849362692369 ) ) ;
#11015 = CARTESIAN_POINT ( 'NONE',  ( -4.592425496802573972E-16, 12.00000000000000178, -7.250000000000000000 ) ) ;
#11016 = CARTESIAN_POINT ( 'NONE',  ( 1.346194077712561166, 9.437500000000003553, -0.2500000000000011102 ) ) ;
#11017 = CARTESIAN_POINT ( 'NONE',  ( 3.249999999999999556, 12.25000000000000000, -3.500000000000000000 ) ) ;
#11018 = ORIENTED_EDGE ( 'NONE', *, *, #12013, .F. ) ;
#11019 = CARTESIAN_POINT ( 'NONE',  ( -60.91137729732986372, 5.000000000000000000, -175.0198515626273661 ) ) ;
#11020 = CARTESIAN_POINT ( 'NONE',  ( 3.249999999999999112, 6.812500000000000000, -2.153805922287439945 ) ) ;
#11021 = CARTESIAN_POINT ( 'NONE',  ( 6.049910241306244885, 5.000000000000000000, -118.3734240199295300 ) ) ;
#11022 = PLANE ( 'NONE',  #11365 ) ;
#11023 = CARTESIAN_POINT ( 'NONE',  ( -40.08271351976077312, 9.999999999999998224, -157.3829028164099668 ) ) ;
#11024 = CARTESIAN_POINT ( 'NONE',  ( 1.266169042200451900, 6.000000000000000000, -139.9015330219193913 ) ) ;
#11025 = ADVANCED_FACE ( 'NONE', ( #7317 ), #874, .F. ) ;
#11026 = PERSON_AND_ORGANIZATION_ROLE ( 'creator' ) ;
#11027 = CARTESIAN_POINT ( 'NONE',  ( 27.95136620086945456, 5.321094445766561876, -28.22695831649836151 ) ) ;
#11028 = ORIENTED_EDGE ( 'NONE', *, *, #8138, .F. ) ;
#11029 = CARTESIAN_POINT ( 'NONE',  ( 3.249999999999999112, 1.812500000000000222, -2.153805922287439945 ) ) ;
#11030 = CARTESIAN_POINT ( 'NONE',  ( -3.749999999999999556, 14.18750000000000000, -1.946699141100892927 ) ) ;
#11031 = ORIENTED_EDGE ( 'NONE', *, *, #9009, .T. ) ;
#11032 = CARTESIAN_POINT ( 'NONE',  ( -3.616507224213203475, -2.490287375297124850, -0.7961248001406434627 ) ) ;
#11033 = CARTESIAN_POINT ( 'NONE',  ( 2.651650429449553759, 2.875000000000000000, -0.8483495705504471296 ) ) ;
#11034 = CARTESIAN_POINT ( 'NONE',  ( 7.669049304201897677, 4.117853033264375462, -21.07967015299796643 ) ) ;
#11035 = CARTESIAN_POINT ( 'NONE',  ( 13.95473576866137755, 13.06343050236333170, -126.2896892777352633 ) ) ;
#11036 = CIRCLE ( 'NONE', #4146, 16.00000000006737721 ) ;
#11037 = CARTESIAN_POINT ( 'NONE',  ( -3.750000000000000000, 2.187500000000000444, -1.946699141100892927 ) ) ;
#11038 = EDGE_CURVE ( 'NONE', #6652, #11706, #13444, .T. ) ;
#11039 = CALENDAR_DATE ( 2026, 8, 10 ) ;
#11040 = CARTESIAN_POINT ( 'NONE',  ( 8.673617379884035472E-16, 9.999999999999998224, -1.663700395152567513 ) ) ;
#11041 = CARTESIAN_POINT ( 'NONE',  ( -0.3766621274091715987, -0.2500000000000000000, -0.1347136637304948981 ) ) ;
#11042 = EDGE_LOOP ( 'NONE', ( #4189, #4529, #11943, #7119, #9162, #8948, #858, #8363 ) ) ;
#11043 = CARTESIAN_POINT ( 'NONE',  ( -2.298097038856278473, 8.125000000000000000, -1.201902961143720416 ) ) ;
#11044 = CARTESIAN_POINT ( 'NONE',  ( -7.920839475687911246, 0.2897469122124984864, -104.3814272194790789 ) ) ;
#11045 = CARTESIAN_POINT ( 'NONE',  ( 1.346194077712558057, 13.56250000000000000, -6.750000000000000000 ) ) ;
#11046 = CARTESIAN_POINT ( 'NONE',  ( -2.298097038856279362, 9.875000000000000000, -5.798097038856278473 ) ) ;
#11047 = CARTESIAN_POINT ( 'NONE',  ( -8.998617940277251037, 9.999999999999998224, -105.4241616556761727 ) ) ;
#11048 = DIRECTION ( 'NONE',  ( 0.000000000000000000, 1.000000000000000000, 0.000000000000000000 ) ) ;
#11049 = DIRECTION ( 'NONE',  ( 0.9961255586397056438, -0.000000000000000000, -0.08794243244722428632 ) ) ;
#11050 = CARTESIAN_POINT ( 'NONE',  ( 2.298097038856278473, 3.625000000000000000, -5.798097038856279362 ) ) ;
#11051 = CARTESIAN_POINT ( 'NONE',  ( 3.749999999999998668, 7.187500000000000888, -5.053300858899108405 ) ) ;
#11052 = CARTESIAN_POINT ( 'NONE',  ( -2.651650429449553314, 8.375000000000000000, -6.151650429449552426 ) ) ;
#11053 = CARTESIAN_POINT ( 'NONE',  ( -3.334720899819473949, 10.18877393819426302, -43.92196855012799972 ) ) ;
#11054 = CARTESIAN_POINT ( 'NONE',  ( 1.553300858899105963, 7.062500000000000888, -7.250000000000000888 ) ) ;
#11055 = CARTESIAN_POINT ( 'NONE',  ( 5.000000000000001776, 1.301042606982605321E-15, -45.97309604003013561 ) ) ;
#11056 = CARTESIAN_POINT ( 'NONE',  ( 11.86629858958631978, 1.298284280918086342, -165.2423957076782131 ) ) ;
#11057 = CARTESIAN_POINT ( 'NONE',  ( 7.497075793982918235, 10.85333879869827456, -25.24968775269402244 ) ) ;
#11058 = CARTESIAN_POINT ( 'NONE',  ( -10.47572155697075402, 1.591638444933427977E-16, -150.0444545769670412 ) ) ;
#11059 = CARTESIAN_POINT ( 'NONE',  ( 0.5944212552585367293, 5.000000000000000888, -138.5540974747773930 ) ) ;
#11060 = CARTESIAN_POINT ( 'NONE',  ( -24.73733098891339210, 8.673617379884034486E-16, -183.9739661531728245 ) ) ;
#11061 = ORIENTED_EDGE ( 'NONE', *, *, #8440, .T. ) ;
#11062 = CARTESIAN_POINT ( 'NONE',  ( -1.346194077712559167, -0.06249999999999988898, -6.749999999999999112 ) ) ;
#11063 = ORIENTED_EDGE ( 'NONE', *, *, #9427, .F. ) ;
#11064 = DIRECTION ( 'NONE',  ( 0.000000000000000000, 0.000000000000000000, -1.000000000000000000 ) ) ;
#11065 = FACE_OUTER_BOUND ( 'NONE', #11484, .T. ) ;
#11066 = CARTESIAN_POINT ( 'NONE',  ( 0.000000000000000000, 9.000000000000001776, 0.2500000000000002220 ) ) ;
#11067 = CARTESIAN_POINT ( 'NONE',  ( 0.000000000000000000, 9.500000000000001776, 0.2499999999999998057 ) ) ;
#11068 = DIRECTION ( 'NONE',  ( 0.000000000000000000, 0.000000000000000000, -1.000000000000000000 ) ) ;
#11069 = ORIENTED_EDGE ( 'NONE', *, *, #6310, .F. ) ;
#11070 = CARTESIAN_POINT ( 'NONE',  ( 3.249999999999998224, 8.312500000000003553, -2.153805922287439945 ) ) ;
#11071 = CARTESIAN_POINT ( 'NONE',  ( -4.592425496802573972E-16, 10.50000000000000000, -7.249999999999999112 ) ) ;
#11072 = CARTESIAN_POINT ( 'NONE',  ( -65.05375779891798516, 15.00000000000000000, -194.1897728445700011 ) ) ;
#11073 = CARTESIAN_POINT ( 'NONE',  ( 0.000000000000000000, 0.000000000000000000, 0.000000000000000000 ) ) ;
#11074 = CARTESIAN_POINT ( 'NONE',  ( 3.249999999999999112, 7.812500000000000000, -2.153805922287439945 ) ) ;
#11075 = CARTESIAN_POINT ( 'NONE',  ( 7.148068729939693000, 2.490287375297123962, -34.56909192082981974 ) ) ;
#11076 = CARTESIAN_POINT ( 'NONE',  ( 0.000000000000000000, -0.2006112523677016091, 0.1491815183709511716 ) ) ;
#11077 = CARTESIAN_POINT ( 'NONE',  ( 3.551824805805253060, 8.673617379884035472E-16, -116.7502625731503656 ) ) ;
#11078 = CARTESIAN_POINT ( 'NONE',  ( 7.000000000000000888, 5.000000000000000888, -1.663700395152567513 ) ) ;
#11079 = DIRECTION ( 'NONE',  ( -0.5427142158096631697, -0.8090169943749466741, 0.2257272309018785728 ) ) ;
#11080 = ORIENTED_EDGE ( 'NONE', *, *, #6390, .T. ) ;
#11081 = DIRECTION ( 'NONE',  ( 0.000000000000000000, 0.000000000000000000, -1.000000000000000000 ) ) ;
#11082 = CARTESIAN_POINT ( 'NONE',  ( 0.3766621274091715987, 0.2956834184403337451, -6.863050255469942407 ) ) ;
#11083 = CARTESIAN_POINT ( 'NONE',  ( -1.553300858899107073, 11.93750000000000178, -7.249999999999999112 ) ) ;
#11084 = CARTESIAN_POINT ( 'NONE',  ( 1.346194077712558279, 10.06250000000000000, -6.750000000000000888 ) ) ;
#11085 = AXIS2_PLACEMENT_3D ( 'NONE', #4799, #7098, #3795 ) ;
#11086 = CARTESIAN_POINT ( 'NONE',  ( -1.346194077712559389, 1.437500000000000000, -6.749999999999999112 ) ) ;
#11087 = ORIENTED_EDGE ( 'NONE', *, *, #12052, .F. ) ;
#11088 = CARTESIAN_POINT ( 'NONE',  ( -2.298097038856278918, 7.375000000000000888, -5.798097038856277585 ) ) ;
#11089 = DIRECTION ( 'NONE',  ( 0.000000000000000000, 0.000000000000000000, -1.000000000000000000 ) ) ;
#11090 = CARTESIAN_POINT ( 'NONE',  ( 13.78275167297412906, 13.34157715675068623, -126.2206732457524794 ) ) ;
#11091 = CARTESIAN_POINT ( 'NONE',  ( 0.4711736884522539359, 9.999999999999998224, 5.336993082470237404 ) ) ;
#11092 = CARTESIAN_POINT ( 'NONE',  ( -47.17052904438269678, 15.00000000000000178, -155.5945877827988113 ) ) ;
#11093 = CALENDAR_DATE ( 2026, 8, 10 ) ;
#11094 = CARTESIAN_POINT ( 'NONE',  ( -25.82983890416511841, 9.999999999999998224, -142.4527639562402328 ) ) ;
#11095 = VERTEX_POINT ( 'NONE', #11108 ) ;
#11096 = CARTESIAN_POINT ( 'NONE',  ( -3.249999999999999112, 13.81250000000000178, -4.846194077712558723 ) ) ;
#11097 = CARTESIAN_POINT ( 'NONE',  ( -3.749999999999999556, 12.31250000000000000, -5.053300858899104853 ) ) ;
#11098 = ORIENTED_EDGE ( 'NONE', *, *, #9004, .T. ) ;
#11099 = SECURITY_CLASSIFICATION ( '', '', #15224 ) ;
#11100 = EDGE_CURVE ( 'NONE', #10578, #14034, #5226, .T. ) ;
#11101 = CARTESIAN_POINT ( 'NONE',  ( -9.836272398077403167, 1.921202954650395256, -34.71741284551207229 ) ) ;
#11102 = CARTESIAN_POINT ( 'NONE',  ( 2.651650429449553759, 0.8750000000000000000, -0.8483495705504471296 ) ) ;
#11103 = CARTESIAN_POINT ( 'NONE',  ( 7.583870713991609946, 3.811257878336620664, -21.41114937039851540 ) ) ;
#11104 = CARTESIAN_POINT ( 'NONE',  ( 0.4075758588480595246, 1.777155427843639446, 4.616619290435463263 ) ) ;
#11105 = CARTESIAN_POINT ( 'NONE',  ( -1.553300858899107073, 2.437500000000000444, -7.250000000000000000 ) ) ;
#11106 = COORDINATED_UNIVERSAL_TIME_OFFSET ( 0, 0, .AHEAD. ) ;
#11107 = LOCAL_TIME ( 12, 28, 20.00000000000000000, #8360 ) ;
#11108 = CARTESIAN_POINT ( 'NONE',  ( 51.19063959271458231, 1.750000000000000000, 71.90077549228632847 ) ) ;
#11109 = FACE_OUTER_BOUND ( 'NONE', #12640, .T. ) ;
#11110 = VECTOR ( 'NONE', #8459, 1000.000000000000227 ) ;
#11111 = ORIENTED_EDGE ( 'NONE', *, *, #1604, .F. ) ;
#11112 = CARTESIAN_POINT ( 'NONE',  ( 0.000000000000000000, 8.000000000000000000, -0.2500000000000002220 ) ) ;
#11113 = CARTESIAN_POINT ( 'NONE',  ( -67.93149434159937528, 9.999999999999998224, -203.8702428815593635 ) ) ;
#11114 = CARTESIAN_POINT ( 'NONE',  ( 3.249999999999998224, 2.187500000000000000, -4.846194077712561388 ) ) ;
#11115 = EDGE_CURVE ( 'NONE', #9540, #4565, #9074, .T. ) ;
#11116 = CARTESIAN_POINT ( 'NONE',  ( 3.249999999999999556, 11.25000000000000000, -3.500000000000000000 ) ) ;
#11117 = DIRECTION ( 'NONE',  ( -0.9961255586397055328, 0.000000000000000000, 0.08794243244722427244 ) ) ;
#11118 = EDGE_CURVE ( 'NONE', #8933, #13770, #10229, .T. ) ;
#11119 = EDGE_CURVE ( 'NONE', #14114, #12741, #5090, .T. ) ;
#11120 = AXIS2_PLACEMENT_3D ( 'NONE', #11843, #10614, #10695 ) ;
#11121 = CARTESIAN_POINT ( 'NONE',  ( -11.47368464578246794, -7.930776467238262242E-13, -126.3895689753432094 ) ) ;
#11122 = CARTESIAN_POINT ( 'NONE',  ( 3.249999999999999556, 6.750000000000000000, -3.500000000000000000 ) ) ;
#11123 = CIRCLE ( 'NONE', #7151, 2.000000000000011546 ) ;
#11124 = CARTESIAN_POINT ( 'NONE',  ( 2.651650429449553314, 6.374999999999999112, -0.8483495705504476847 ) ) ;
#11125 = AXIS2_PLACEMENT_3D ( 'NONE', #13614, #12436, #7866 ) ;
#11126 = CIRCLE ( 'NONE', #9152, 10.00000000000000888 ) ;
#11127 = CARTESIAN_POINT ( 'NONE',  ( 3.749999999999999112, 10.68750000000000000, -5.053300858899108405 ) ) ;
#11128 = CARTESIAN_POINT ( 'NONE',  ( 11.04730217088350663, 15.00000000000000000, -107.1178495010082941 ) ) ;
#11129 = CARTESIAN_POINT ( 'NONE',  ( 0.1865371907817764130, 3.106934502706220957, 2.112910209604430545 ) ) ;
#11130 = CARTESIAN_POINT ( 'NONE',  ( 1.553300858899109516, 10.43750000000000178, 0.2499999999999993616 ) ) ;
#11131 = CARTESIAN_POINT ( 'NONE',  ( -25.66911763371813038, 15.00000000000000000, -138.9799121221676046 ) ) ;
#11132 = CARTESIAN_POINT ( 'NONE',  ( 12.06072315356882996, 1.933739209393280589, -165.9530378701809923 ) ) ;
#11133 = CARTESIAN_POINT ( 'NONE',  ( 34.65560150440948206, 2.100000000001073008, 38.24242331140461459 ) ) ;
#11134 = CONICAL_SURFACE ( 'NONE', #10160, 0.4999999999999865663, 0.6283185307179600665 ) ;
#11135 = CARTESIAN_POINT ( 'NONE',  ( -24.39793690352481548, 0.000000000000000000, -182.5284601783003495 ) ) ;
#11136 = DIRECTION ( 'NONE',  ( 0.000000000000000000, 1.000000000000000000, 0.000000000000000000 ) ) ;
#11137 = UNCERTAINTY_MEASURE_WITH_UNIT (LENGTH_MEASURE( 1.000000000000000082E-05 ), #1419, 'distance_accuracy_value', 'NONE');
#11138 = CARTESIAN_POINT ( 'NONE',  ( -47.43378631392564415, 15.00000000000000000, -155.7534628402561339 ) ) ;
#11139 = CARTESIAN_POINT ( 'NONE',  ( -3.750000000000000000, 13.81250000000000178, -5.053300858899105741 ) ) ;
#11140 = VERTEX_POINT ( 'NONE', #11040 ) ;
#11141 = FACE_BOUND ( 'NONE', #4687, .T. ) ;
#11142 = FACE_OUTER_BOUND ( 'NONE', #15070, .T. ) ;
#11143 = CARTESIAN_POINT ( 'NONE',  ( -2.651650429449553314, 11.37500000000000000, -6.151650429449552426 ) ) ;
#11144 = CARTESIAN_POINT ( 'NONE',  ( 1.553300858899109071, 6.437499999999999112, 0.2499999999999989175 ) ) ;
#11145 = CARTESIAN_POINT ( 'NONE',  ( 25.37742002255717466, 1.750000000000000000, 70.49803269364883818 ) ) ;
#11146 = CC_DESIGN_PERSON_AND_ORGANIZATION_ASSIGNMENT ( #5542, #6550, ( #13819 ) ) ;
#11147 = CARTESIAN_POINT ( 'NONE',  ( -9.625715240929041627, 3.489827457201579275, -115.8367759348243595 ) ) ;
#11148 = CARTESIAN_POINT ( 'NONE',  ( 0.000000000000000000, 7.499999999999999112, -0.2500000000000002220 ) ) ;
#11149 = CARTESIAN_POINT ( 'NONE',  ( -4.592425496802573972E-16, 1.084202172485504434E-16, -7.250000000000000000 ) ) ;
#11150 = CARTESIAN_POINT ( 'NONE',  ( -64.05876861121487309, 15.00000000000000000, -200.0474132877887996 ) ) ;
#11151 = DIRECTION ( 'NONE',  ( 0.000000000000000000, 0.000000000000000000, 1.000000000000000000 ) ) ;
#11152 = DIRECTION ( 'NONE',  ( 1.000000000000000000, 0.000000000000000000, 0.000000000000000000 ) ) ;
#11153 = CARTESIAN_POINT ( 'NONE',  ( -2.298097038856278473, 10.12500000000000000, -1.201902961143720416 ) ) ;
#11154 = DIRECTION ( 'NONE',  ( 0.002879925520667554837, 0.000000000000000000, 0.9999958530058988826 ) ) ;
#11155 = CARTESIAN_POINT ( 'NONE',  ( 0.000000000000000000, 5.000000000000000000, 0.000000000000000000 ) ) ;
#11156 = CARTESIAN_POINT ( 'NONE',  ( 8.873074003806229015, 1.073784846296689040E-12, -110.5883967389756748 ) ) ;
#11157 = CARTESIAN_POINT ( 'NONE',  ( -10.29275726619092524, 0.000000000000000000, -34.56909192082969184 ) ) ;
#11158 = DIRECTION ( 'NONE',  ( 0.7779936141972743080, 0.000000000000000000, 0.6282721832679390994 ) ) ;
#11159 = ORIENTED_EDGE ( 'NONE', *, *, #9620, .F. ) ;
#11160 = FACE_OUTER_BOUND ( 'NONE', #3620, .T. ) ;
#11161 = CARTESIAN_POINT ( 'NONE',  ( 4.413686865555820127, 15.00000000000000178, -104.6754972201258482 ) ) ;
#11162 = CARTESIAN_POINT ( 'NONE',  ( 1.553300858899105963, 14.06250000000000178, -7.249999999999999112 ) ) ;
#11163 = CARTESIAN_POINT ( 'NONE',  ( -2.298097038856278029, 9.624999999999998224, -1.201902961143720638 ) ) ;
#11164 = CARTESIAN_POINT ( 'NONE',  ( 0.000000000000000000, 14.50000000000000000, -0.2500000000000002220 ) ) ;
#11165 = ORIENTED_EDGE ( 'NONE', *, *, #1678, .F. ) ;
#11166 = CARTESIAN_POINT ( 'NONE',  ( 2.298097038856279362, 12.87500000000000178, -1.201902961143720860 ) ) ;
#11167 = CARTESIAN_POINT ( 'NONE',  ( -6.749805820977427651, 0.000000000000000000, -104.8828629986478518 ) ) ;
#11168 = LOCAL_TIME ( 12, 28, 20.00000000000000000, #5390 ) ;
#11169 = CARTESIAN_POINT ( 'NONE',  ( 9.969654309237004242, 12.69562645089776964, -44.87941232917236789 ) ) ;
#11170 = FACE_OUTER_BOUND ( 'NONE', #4407, .T. ) ;
#11171 = CARTESIAN_POINT ( 'NONE',  ( 17.50071171097425804, 8.749999999999998224, -91.70093451412481045 ) ) ;
#11172 = DATE_AND_TIME ( #11093, #12578 ) ;
#11173 = FACE_OUTER_BOUND ( 'NONE', #14404, .T. ) ;
#11174 = AXIS2_PLACEMENT_3D ( 'NONE', #13567, #15037, #5295 ) ;
#11175 = VERTEX_POINT ( 'NONE', #6395 ) ;
#11176 = CARTESIAN_POINT ( 'NONE',  ( -1.346194077712559389, 4.437500000000000888, -6.749999999999999112 ) ) ;
#11177 = CARTESIAN_POINT ( 'NONE',  ( -4.592425496802573972E-16, 11.50000000000000000, -7.249999999999999112 ) ) ;
#11178 = ORIENTED_EDGE ( 'NONE', *, *, #12261, .T. ) ;
#11179 = DIRECTION ( 'NONE',  ( -0.000000000000000000, -1.000000000000000000, -0.000000000000000000 ) ) ;
#11180 = CARTESIAN_POINT ( 'NONE',  ( 3.750000000000000000, 2.750000000000000000, -3.500000000000000444 ) ) ;
#11181 = AXIS2_PLACEMENT_3D ( 'NONE', #13983, #8951, #13681 ) ;
#11182 = DIRECTION ( 'NONE',  ( 0.000000000000000000, 1.000000000000000000, 0.000000000000000000 ) ) ;
#11183 = CARTESIAN_POINT ( 'NONE',  ( 0.5065669486108499431, 4.652565967668215841, 5.737893194806527042 ) ) ;
#11184 = CARTESIAN_POINT ( 'NONE',  ( -3.750000000000000000, 0.1875000000000000555, -1.946699141100892927 ) ) ;
#11185 = PERSON_AND_ORGANIZATION ( #3176, #3020 ) ;
#11186 = ADVANCED_FACE ( 'NONE', ( #6246 ), #232, .F. ) ;
#11187 = PLANE ( 'NONE',  #10706 ) ;
#11188 = CARTESIAN_POINT ( 'NONE',  ( -3.249999999999999556, 11.25000000000000000, -3.499999999999999556 ) ) ;
#11189 = DIRECTION ( 'NONE',  ( -0.000000000000000000, -0.000000000000000000, 1.000000000000000000 ) ) ;
#11190 = EDGE_LOOP ( 'NONE', ( #14031, #6530, #8128, #4958 ) ) ;
#11191 = CARTESIAN_POINT ( 'NONE',  ( -3.980102097228897245E-16, 9.500000000000000000, -6.749999999999999112 ) ) ;
#11192 = AXIS2_PLACEMENT_3D ( 'NONE', #4434, #9145, #13949 ) ;
#11193 = CARTESIAN_POINT ( 'NONE',  ( -4.234402844927150689, 15.00000000000000000, -117.4888040839639558 ) ) ;
#11194 = VECTOR ( 'NONE', #8451, 1000.000000000000000 ) ;
#11195 = CARTESIAN_POINT ( 'NONE',  ( -3.249999999999999112, 4.687500000000000000, -2.153805922287440833 ) ) ;
#11196 = CARTESIAN_POINT ( 'NONE',  ( 1.346194077712558279, 10.06250000000000000, -6.750000000000000888 ) ) ;
#11197 = CARTESIAN_POINT ( 'NONE',  ( -0.1117941955214300648, 10.00000000000000000, -102.1231258608400907 ) ) ;
#11198 = CC_DESIGN_PERSON_AND_ORGANIZATION_ASSIGNMENT ( #4092, #14990, ( #8425 ) ) ;
#11199 = DIRECTION ( 'NONE',  ( 1.000000000000000000, 0.000000000000000000, 0.000000000000000000 ) ) ;
#11200 = CARTESIAN_POINT ( 'NONE',  ( 2.298097038856278473, 4.625000000000000000, -5.798097038856279362 ) ) ;
#11201 = CARTESIAN_POINT ( 'NONE',  ( -4.592425496802573972E-16, 4.000000000000000000, -7.250000000000000000 ) ) ;
#11202 = CARTESIAN_POINT ( 'NONE',  ( -1.553300858899106407, 9.062500000000000000, 0.2500000000000002220 ) ) ;
#11203 = CARTESIAN_POINT ( 'NONE',  ( 0.2499999999999999445, 4.500000000000000888, 1.500000000000000222 ) ) ;
#11204 = VERTEX_POINT ( 'NONE', #4166 ) ;
#11205 = CARTESIAN_POINT ( 'NONE',  ( -9.385448347264267355, 9.999999999999998224, -115.3551636530117150 ) ) ;
#11206 = CARTESIAN_POINT ( 'NONE',  ( 2.651650429449554203, 8.375000000000000000, -0.8483495705504471296 ) ) ;
#11207 = CIRCLE ( 'NONE', #2328, 2.271449424009384987 ) ;
#11208 = CARTESIAN_POINT ( 'NONE',  ( 3.891364641103005617, 14.90536770052132098, -1.768596708628414449 ) ) ;
#11209 = CARTESIAN_POINT ( 'NONE',  ( 6.369258321017760238, -2.075239479414269894, -34.56909192082981974 ) ) ;
#11210 = ADVANCED_FACE ( 'NONE', ( #7628 ), #8868, .F. ) ;
#11211 = ADVANCED_FACE ( 'NONE', ( #6470 ), #11187, .T. ) ;
#11212 = CARTESIAN_POINT ( 'NONE',  ( 5.354258359986379112, 2.100000000000000089, 6.532454833391891036 ) ) ;
#11213 = CARTESIAN_POINT ( 'NONE',  ( -20.78318744499695470, 8.673617379884035472E-16, -172.3918248695773059 ) ) ;
#11214 = LINE ( 'NONE', #11438, #6927 ) ;
#11215 = CARTESIAN_POINT ( 'NONE',  ( -43.45407652371731189, 15.00000000000000000, -153.4178398490312532 ) ) ;
#11216 = CARTESIAN_POINT ( 'NONE',  ( -2.651650429449553314, 11.87500000000000000, -6.151650429449552426 ) ) ;
#11217 = EDGE_LOOP ( 'NONE', ( #11842, #13603, #1180, #1811, #8022, #5403 ) ) ;
#11218 = FACE_OUTER_BOUND ( 'NONE', #5361, .T. ) ;
#11219 = FACE_OUTER_BOUND ( 'NONE', #6118, .T. ) ;
#11220 = CIRCLE ( 'NONE', #4556, 3.500000000000000000 ) ;
#11221 = CARTESIAN_POINT ( 'NONE',  ( -4.592425496802573972E-16, 7.000000000000000000, -7.250000000000000000 ) ) ;
#11222 = DIRECTION ( 'NONE',  ( 0.000000000000000000, 0.000000000000000000, -1.000000000000000000 ) ) ;
#11223 = CARTESIAN_POINT ( 'NONE',  ( -8.455319114079472342, 1.782382842817059165, -116.6570696633463911 ) ) ;
#11224 = CARTESIAN_POINT ( 'NONE',  ( 3.249999999999998224, 8.187500000000000000, -4.846194077712561388 ) ) ;
#11225 = CARTESIAN_POINT ( 'NONE',  ( -9.422314331838387957, 0.000000000000000000, -135.7831129423652214 ) ) ;
#11226 = CARTESIAN_POINT ( 'NONE',  ( -1.553300858899107295, 12.43750000000000000, -7.250000000000000000 ) ) ;
#11227 = DIRECTION ( 'NONE',  ( 0.9961255586397055328, -0.000000000000000000, -0.08794243244722428632 ) ) ;
#11228 = CARTESIAN_POINT ( 'NONE',  ( -14.59253236707263213, -1.779437631024875872E-15, -133.7561938577802891 ) ) ;
#11229 = CARTESIAN_POINT ( 'NONE',  ( -2.298097038856278918, 12.37500000000000000, -5.798097038856277585 ) ) ;
#11230 = EDGE_CURVE ( 'NONE', #3740, #5461, #13121, .T. ) ;
#11231 = CARTESIAN_POINT ( 'NONE',  ( -5.090128371569606180, 10.00000000000000178, -112.6869195057500690 ) ) ;
#11232 = B_SPLINE_CURVE_WITH_KNOTS ( 'NONE', 3,
 ( #7903, #10458, #11539, #954 ),
 .UNSPECIFIED., .F., .F.,
 ( 4, 4 ),
 ( -1.414214726962510347E-05, 0.001035133531573338228 ),
 .UNSPECIFIED. ) ;
#11233 = FACE_OUTER_BOUND ( 'NONE', #14679, .T. ) ;
#11234 = DIRECTION ( 'NONE',  ( -0.08794243244722425856, -0.000000000000000000, -0.9961255586397054218 ) ) ;
#11235 = DIRECTION ( 'NONE',  ( 0.02181900108494732801, 0.000000000000000000, -0.9997619372588931741 ) ) ;
#11236 = DIRECTION ( 'NONE',  ( 0.000000000000000000, 0.000000000000000000, 1.000000000000000000 ) ) ;
#11237 = VERTEX_POINT ( 'NONE', #7788 ) ;
#11238 = CARTESIAN_POINT ( 'NONE',  ( 9.952382861741629227, 4.874414676631592336, -43.73669136194838813 ) ) ;
#11239 = CARTESIAN_POINT ( 'NONE',  ( 11.46158717457445242, 12.50000000000000355, -122.9370801587496231 ) ) ;
#11240 = CARTESIAN_POINT ( 'NONE',  ( 2.651650429449553759, 1.875000000000000000, -0.8483495705504471296 ) ) ;
#11241 = CARTESIAN_POINT ( 'NONE',  ( -3.249999999999999556, 11.75000000000000178, -3.500000000000000000 ) ) ;
#11242 = CARTESIAN_POINT ( 'NONE',  ( 3.249999999999998668, 0.6875000000000000000, -4.846194077712560500 ) ) ;
#11243 = ORIENTED_EDGE ( 'NONE', *, *, #14054, .F. ) ;
#11244 = CARTESIAN_POINT ( 'NONE',  ( -1.346194077712559389, 10.06250000000000000, -0.2500000000000002220 ) ) ;
#11245 = DIRECTION ( 'NONE',  ( 0.000000000000000000, 0.000000000000000000, -1.000000000000000000 ) ) ;
#11246 = DIRECTION ( 'NONE',  ( 0.000000000000000000, 0.000000000000000000, -1.000000000000000000 ) ) ;
#11247 = CARTESIAN_POINT ( 'NONE',  ( -25.42939282183900573, 4.000000000000000000, -209.0516719515502473 ) ) ;
#11248 = CARTESIAN_POINT ( 'NONE',  ( -9.131312970615338642, 12.51400246205168010, -116.0049100415184569 ) ) ;
#11249 = PERSON_AND_ORGANIZATION ( #5750, #12097 ) ;
#11250 = CARTESIAN_POINT ( 'NONE',  ( 12.15266112769998053, 15.00000000000000000, -123.9192486815589263 ) ) ;
#11251 = CARTESIAN_POINT ( 'NONE',  ( 27.51230736755065109, 4.535074869370507855, -137.3927180564188006 ) ) ;
#11252 = ORIENTED_EDGE ( 'NONE', *, *, #368, .F. ) ;
#11253 = CARTESIAN_POINT ( 'NONE',  ( 2.298097038856278473, 4.625000000000000000, -5.798097038856279362 ) ) ;
#11254 = CARTESIAN_POINT ( 'NONE',  ( -29.11373319368141921, 4.000000000000000000, -181.2633039353972322 ) ) ;
#11255 = CARTESIAN_POINT ( 'NONE',  ( -4.592425496802573972E-16, 1.084202172485504434E-16, -7.250000000000000000 ) ) ;
#11256 = EDGE_LOOP ( 'NONE', ( #458, #1102, #10995, #9049, #10825, #14021 ) ) ;
#11257 = CARTESIAN_POINT ( 'NONE',  ( -4.598444398438791936, 1.750000000000027311, 31.18418455424690805 ) ) ;
#11258 = CARTESIAN_POINT ( 'NONE',  ( -3.750000000000000000, 3.250000000000000444, -3.499999999999999112 ) ) ;
#11259 = CARTESIAN_POINT ( 'NONE',  ( 9.971950858281140029, 8.773889247172311556, -44.63331069169930032 ) ) ;
#11260 = CARTESIAN_POINT ( 'NONE',  ( 2.889412549072087444, 0.4949020854232912270, 2.410474734309482336 ) ) ;
#11261 = CARTESIAN_POINT ( 'NONE',  ( 3.749999999999999112, 1.687500000000000000, -5.053300858899108405 ) ) ;
#11262 = CALENDAR_DATE ( 2026, 8, 10 ) ;
#11263 = CARTESIAN_POINT ( 'NONE',  ( 11.02460460396801345, 5.000000000000000888, -122.2267226321878866 ) ) ;
#11264 = CARTESIAN_POINT ( 'NONE',  ( 0.5944212552585367293, 0.000000000000000000, -138.5540974747773930 ) ) ;
#11265 = ORIENTED_EDGE ( 'NONE', *, *, #11859, .T. ) ;
#11266 = FACE_OUTER_BOUND ( 'NONE', #9290, .T. ) ;
#11267 = CARTESIAN_POINT ( 'NONE',  ( -2.298097038856278029, 3.625000000000000888, -1.201902961143720638 ) ) ;
#11268 = CARTESIAN_POINT ( 'NONE',  ( 2.298097038856278029, 13.12499999999999822, -5.798097038856279362 ) ) ;
#11269 = ADVANCED_FACE ( 'NONE', ( #7858 ), #13674, .T. ) ;
#11270 = CARTESIAN_POINT ( 'NONE',  ( -8.998617940277251037, 15.00000000000000000, -105.4241616556761585 ) ) ;
#11271 = CARTESIAN_POINT ( 'NONE',  ( 10.73540465342505357, 13.79079921804019548, -106.9347929316625425 ) ) ;
#11272 = EDGE_CURVE ( 'NONE', #788, #13477, #6002, .T. ) ;
#11273 = CARTESIAN_POINT ( 'NONE',  ( 0.000000000000000000, 7.000000000000000000, -0.2500000000000002220 ) ) ;
#11274 = CARTESIAN_POINT ( 'NONE',  ( 1.553300858899109071, 6.437499999999999112, 0.2499999999999989175 ) ) ;
#11275 = CARTESIAN_POINT ( 'NONE',  ( 1.553300858899108849, 9.937499999999998224, 0.2499999999999993616 ) ) ;
#11276 = CIRCLE ( 'NONE', #7316, 3.500000000000003109 ) ;
#11277 = CARTESIAN_POINT ( 'NONE',  ( -0.9087754948914270603, -2.490287375297125294, -36.05536862169275025 ) ) ;
#11278 = CARTESIAN_POINT ( 'NONE',  ( -3.333302013784147810, 9.945430626687967290, -43.56301687292351232 ) ) ;
#11279 = CARTESIAN_POINT ( 'NONE',  ( 2.651650429449554203, 11.37500000000000000, -0.8483495705504471296 ) ) ;
#11280 = CARTESIAN_POINT ( 'NONE',  ( 4.673610763312950667, 0.0002987076048428271343, -16.05876724900730679 ) ) ;
#11281 = CARTESIAN_POINT ( 'NONE',  ( 30.32986759126112730, 0.7500000000000000000, 43.04214087805580391 ) ) ;
#11282 = CARTESIAN_POINT ( 'NONE',  ( 9.861753912003623057, 1.663174471683243949, -106.5437946333974679 ) ) ;
#11283 = ORIENTED_EDGE ( 'NONE', *, *, #4574, .T. ) ;
#11284 = CARTESIAN_POINT ( 'NONE',  ( -22.38002629026897594, -1.081729916803953434E-12, -166.3206558604766201 ) ) ;
#11285 = CARTESIAN_POINT ( 'NONE',  ( 0.000000000000000000, 1.000000000000000000, -0.2500000000000002220 ) ) ;
#11286 = CARTESIAN_POINT ( 'NONE',  ( -48.42971706865863979, 14.99999999999999467, -163.2864622074216356 ) ) ;
#11287 = CARTESIAN_POINT ( 'NONE',  ( 2.298097038856278029, 0.1250000000000001110, -5.798097038856279362 ) ) ;
#11288 = EDGE_LOOP ( 'NONE', ( #11535, #6832, #1956, #2170 ) ) ;
#11289 = DIRECTION ( 'NONE',  ( -0.000000000000000000, -1.000000000000000000, -0.000000000000000000 ) ) ;
#11290 = CYLINDRICAL_SURFACE ( 'NONE', #5772, 3.500000000000013323 ) ;
#11291 = CARTESIAN_POINT ( 'NONE',  ( -8.243994158936983396, 9.999999999999998224, -104.7509493499769917 ) ) ;
#11292 = DIRECTION ( 'NONE',  ( -0.000000000000000000, -1.000000000000000000, -0.000000000000000000 ) ) ;
#11293 = EDGE_CURVE ( 'NONE', #1404, #14984, #8516, .T. ) ;
#11294 = CARTESIAN_POINT ( 'NONE',  ( 1.346194077712561166, 7.437499999999999112, -0.2500000000000011102 ) ) ;
#11295 = DIRECTION ( 'NONE',  ( 0.000000000000000000, 0.000000000000000000, 1.000000000000000000 ) ) ;
#11296 = CARTESIAN_POINT ( 'NONE',  ( 3.749999999999999112, 13.81250000000000000, -1.946699141100892039 ) ) ;
#11297 =( BOUNDED_SURFACE ( )  B_SPLINE_SURFACE ( 3, 2, ( 
 ( #3520, #10553, #12803 ),
 ( #7215, #9391, #13030 ),
 ( #9471, #14197, #12958 ),
 ( #46, #14119, #11711 ),
 ( #4755, #11782, #2208 ),
 ( #8302, #11852, #9319 ),
 ( #8228, #1277, #6916 ),
 ( #10704, #11636, #120 ),
 ( #1054, #3439, #4834 ),
 ( #9546, #8150, #2365 ),
 ( #15219, #7062, #14272 ),
 ( #2291, #8375, #6995 ),
 ( #1129, #14437, #14351 ),
 ( #13430, #13188, #1942 ),
 ( #3914, #3751, #14875 ),
 ( #8535, #6581, #7373 ),
 ( #6302, #10941, #6656 ),
 ( #2754, #11369, #14515 ) ),
 .UNSPECIFIED., .F., .F., .T. ) 
 B_SPLINE_SURFACE_WITH_KNOTS ( ( 4, 2, 2, 2, 2, 2, 2, 2, 4 ),
 ( 3, 3 ),
 ( -2.168404344971008868E-19, 0.002802366342598247659, 0.005604732685196495319, 0.007005915856495618932, 0.008407099027794743412, 0.01120946537039299064, 0.01401183171299123786, 0.01681419805558948682, 0.02241893074078598128 ),
 ( 0.000000000000000000, 1.000000000000000000 ),
 .UNSPECIFIED. ) 
 GEOMETRIC_REPRESENTATION_ITEM ( )  RATIONAL_B_SPLINE_SURFACE ( (
 ( 1.000000000000000000, 0.7071067811865475727, 1.000000000000000000),
 ( 1.000000000000000000, 0.7071067811865475727, 1.000000000000000000),
 ( 1.000000000000000000, 0.7071067811865475727, 1.000000000000000000),
 ( 1.000000000000000000, 0.7071067811865475727, 1.000000000000000000),
 ( 1.000000000000000000, 0.7071067811865475727, 1.000000000000000000),
 ( 1.000000000000000000, 0.7071067811865475727, 1.000000000000000000),
 ( 1.000000000000000000, 0.7071067811865474617, 1.000000000000000000),
 ( 1.000000000000000000, 0.7071067811865474617, 1.000000000000000000),
 ( 1.000000000000000000, 0.7071067811865475727, 1.000000000000000000),
 ( 1.000000000000000000, 0.7071067811865475727, 1.000000000000000000),
 ( 1.000000000000000000, 0.7071067811865475727, 1.000000000000000000),
 ( 1.000000000000000000, 0.7071067811865475727, 1.000000000000000000),
 ( 1.000000000000000000, 0.7071067811865475727, 1.000000000000000000),
 ( 1.000000000000000000, 0.7071067811865475727, 1.000000000000000000),
 ( 1.000000000000000000, 0.7071067811865475727, 1.000000000000000000),
 ( 1.000000000000000000, 0.7071067811865475727, 1.000000000000000000),
 ( 1.000000000000000000, 0.7071067811865474617, 1.000000000000000000),
 ( 1.000000000000000000, 0.7071067811865474617, 1.000000000000000000) ) ) 
 REPRESENTATION_ITEM ( '' )  SURFACE ( )  );
#11298 = CYLINDRICAL_SURFACE ( 'NONE', #10147, 3.000000000000010214 ) ;
#11299 = DIRECTION ( 'NONE',  ( 0.000000000000000000, 0.000000000000000000, -1.000000000000000000 ) ) ;
#11300 = CARTESIAN_POINT ( 'NONE',  ( 3.249999999999999556, 10.75000000000000000, -3.500000000000000000 ) ) ;
#11301 = CARTESIAN_POINT ( 'NONE',  ( -0.3766621274091715987, 0.2858031308077496613, -0.04317668481647501943 ) ) ;
#11302 = DIRECTION ( 'NONE',  ( -0.02181900108494707127, -0.000000000000000000, 0.9997619372588931741 ) ) ;
#11303 = CARTESIAN_POINT ( 'NONE',  ( -2.298097038856278918, 8.375000000000000000, -5.798097038856277585 ) ) ;
#11304 = CARTESIAN_POINT ( 'NONE',  ( 2.553779201801159804, 8.673617379884035472E-16, -128.9691103915868382 ) ) ;
#11305 = DIRECTION ( 'NONE',  ( -0.9876883405951377704, 0.000000000000000000, -0.1564344650402312575 ) ) ;
#11306 = CC_DESIGN_DATE_AND_TIME_ASSIGNMENT ( #4521, #8065, ( #3971 ) ) ;
#11307 = ORIENTED_EDGE ( 'NONE', *, *, #11565, .T. ) ;
#11308 = CARTESIAN_POINT ( 'NONE',  ( 7.781170200712294260, 5.000000000000000888, -20.49502329017444424 ) ) ;
#11309 = CARTESIAN_POINT ( 'NONE',  ( -5.613243360039387397, 3.999999999999999112, -181.6031318735493869 ) ) ;
#11310 = CARTESIAN_POINT ( 'NONE',  ( -3.749999999999999556, 1.312500000000000444, -5.053300858899104853 ) ) ;
#11311 = CARTESIAN_POINT ( 'NONE',  ( 1.346194077712561166, 15.43750000000000178, -0.2500000000000011102 ) ) ;
#11312 = CARTESIAN_POINT ( 'NONE',  ( -1.346194077712559389, 1.062500000000000222, -0.2500000000000002220 ) ) ;
#11313 = EDGE_LOOP ( 'NONE', ( #6457, #6622, #7366, #6193 ) ) ;
#11314 = EDGE_CURVE ( 'NONE', #3493, #4119, #11419, .T. ) ;
#11315 = CARTESIAN_POINT ( 'NONE',  ( -1.346194077712559389, 12.43750000000000000, -6.749999999999999112 ) ) ;
#11316 = EDGE_CURVE ( 'NONE', #8744, #3728, #7241, .T. ) ;
#11317 = ADVANCED_FACE ( 'NONE', ( #12656 ), #2071, .F. ) ;
#11318 = FACE_OUTER_BOUND ( 'NONE', #14171, .T. ) ;
#11319 = CYLINDRICAL_SURFACE ( 'NONE', #11641, 14.80000000000025651 ) ;
#11320 = CARTESIAN_POINT ( 'NONE',  ( -4.890501715614027134, 14.99999999916422233, -117.3116236002413899 ) ) ;
#11321 = DATE_AND_TIME ( #3057, #241 ) ;
#11322 = CARTESIAN_POINT ( 'NONE',  ( 8.507048280578556998, 15.00000000000000000, -111.8750672986241881 ) ) ;
#11323 = CARTESIAN_POINT ( 'NONE',  ( -9.681086997240701209, 10.70057783228466519, -116.3713800322179850 ) ) ;
#11324 = VECTOR ( 'NONE', #8270, 1000.000000000000227 ) ;
#11325 = CARTESIAN_POINT ( 'NONE',  ( 3.158384440324536246, -0.4889170748306868597, -1.000000000000001554 ) ) ;
#11326 = ORIENTED_EDGE ( 'NONE', *, *, #1384, .T. ) ;
#11327 = CARTESIAN_POINT ( 'NONE',  ( -2.298097038856278918, 5.375000000000000000, -5.798097038856277585 ) ) ;
#11328 = CARTESIAN_POINT ( 'NONE',  ( -29.51097267919375611, 4.000000000000000888, -182.9257734226692378 ) ) ;
#11329 = CARTESIAN_POINT ( 'NONE',  ( 3.749999999999999112, 2.187500000000000000, -5.053300858899108405 ) ) ;
#11330 = ORIENTED_EDGE ( 'NONE', *, *, #3374, .F. ) ;
#11331 = CARTESIAN_POINT ( 'NONE',  ( -8.648486276335452416, 12.61601666265212529, -115.6868502166757224 ) ) ;
#11332 = CARTESIAN_POINT ( 'NONE',  ( -4.592425496802573972E-16, 4.500000000000000888, -7.249999999999999112 ) ) ;
#11333 = CARTESIAN_POINT ( 'NONE',  ( 30.32986759126112730, 0.7500000000000000000, 39.54214087805579680 ) ) ;
#11334 = CARTESIAN_POINT ( 'NONE',  ( 2.595281665815428518, 9.245940400502809730E-16, 0.5467206721942569070 ) ) ;
#11335 = CARTESIAN_POINT ( 'NONE',  ( 3.749999999999999556, 0.8125000000000001110, -1.946699141100892261 ) ) ;
#11336 = SECURITY_CLASSIFICATION_LEVEL ( 'unclassified' ) ;
#11337 = CARTESIAN_POINT ( 'NONE',  ( -4.365898909102353009, 1.829703814864835687, -1.000000000000011546 ) ) ;
#11338 = CARTESIAN_POINT ( 'NONE',  ( -3.249999999999999556, 11.18749999999999822, -2.153805922287440833 ) ) ;
#11339 = ORIENTED_EDGE ( 'NONE', *, *, #412, .F. ) ;
#11340 = CARTESIAN_POINT ( 'NONE',  ( -35.61761402690549261, 15.00000000000000178, -151.2353583422565748 ) ) ;
#11341 = CARTESIAN_POINT ( 'NONE',  ( 1.346194077712558279, 3.062500000000000000, -6.750000000000000888 ) ) ;
#11342 = FACE_OUTER_BOUND ( 'NONE', #1276, .T. ) ;
#11343 = CARTESIAN_POINT ( 'NONE',  ( -5.616965975805494615, 4.336808689942017736E-16, -122.7637103460384935 ) ) ;
#11344 = CARTESIAN_POINT ( 'NONE',  ( 0.000000000000000000, 4.499999999999999112, 0.2499999999999998057 ) ) ;
#11345 = CARTESIAN_POINT ( 'NONE',  ( 1.553300858899108849, 7.937500000000000000, 0.2499999999999993616 ) ) ;
#11346 = LOCAL_TIME ( 12, 28, 20.00000000000000000, #4080 ) ;
#11347 = CARTESIAN_POINT ( 'NONE',  ( -2.869987474717049292, 2.165641995257062025, -1.000000000000004663 ) ) ;
#11348 = VERTEX_POINT ( 'NONE', #9551 ) ;
#11349 = DIRECTION ( 'NONE',  ( 1.000000000000000000, 0.000000000000000000, 0.000000000000000000 ) ) ;
#11350 = CARTESIAN_POINT ( 'NONE',  ( -4.592425496802573972E-16, 12.00000000000000178, -7.250000000000000000 ) ) ;
#11351 = LINE ( 'NONE', #8960, #5765 ) ;
#11352 = AXIS2_PLACEMENT_3D ( 'NONE', #8602, #1726, #14505 ) ;
#11353 = DIRECTION ( 'NONE',  ( -0.000000000000000000, -1.000000000000000000, -0.000000000000000000 ) ) ;
#11354 = DIRECTION ( 'NONE',  ( 0.000000000000000000, 0.000000000000000000, 1.000000000000000000 ) ) ;
#11355 = VERTEX_POINT ( 'NONE', #9628 ) ;
#11356 = CARTESIAN_POINT ( 'NONE',  ( -18.78509308054654170, 8.673617379884035472E-16, -168.2639965131413931 ) ) ;
#11357 = CARTESIAN_POINT ( 'NONE',  ( 11.61481609544922655, 1.294168654864739310, -165.5398345278520651 ) ) ;
#11358 = CARTESIAN_POINT ( 'NONE',  ( -47.49849438536951141, 14.99999999999460520, -162.3383809241247491 ) ) ;
#11359 = APPROVAL_PERSON_ORGANIZATION ( #420, #6490, #1575 ) ;
#11360 = CARTESIAN_POINT ( 'NONE',  ( 1.346194077712558279, 4.062500000000001776, -6.750000000000000888 ) ) ;
#11361 = EDGE_LOOP ( 'NONE', ( #5733, #3264, #9177, #704, #14325, #5955 ) ) ;
#11362 = FACE_OUTER_BOUND ( 'NONE', #15133, .T. ) ;
#11363 = AXIS2_PLACEMENT_3D ( 'NONE', #12674, #3094, #4338 ) ;
#11364 = CARTESIAN_POINT ( 'NONE',  ( 7.148068729939690336, -2.490287375297125294, -34.56909192082981974 ) ) ;
#11365 = AXIS2_PLACEMENT_3D ( 'NONE', #14751, #6378, #12255 ) ;
#11366 = CARTESIAN_POINT ( 'NONE',  ( 26.73766085848597740, 6.000000000000000000, -138.7442440334353080 ) ) ;
#11367 = VECTOR ( 'NONE', #3857, 1000.000000000000000 ) ;
#11368 = CARTESIAN_POINT ( 'NONE',  ( -3.249999999999999556, 10.31250000000000000, -4.846194077712557835 ) ) ;
#11369 = CARTESIAN_POINT ( 'NONE',  ( -9.476787056091273698, 15.00000000000000000, -115.4301398046334839 ) ) ;
#11370 = CARTESIAN_POINT ( 'NONE',  ( -6.992168204854784186, 5.000000000000000888, -113.2636094675863063 ) ) ;
#11371 = CARTESIAN_POINT ( 'NONE',  ( -1.346194077712559167, 9.937500000000001776, -6.749999999999999112 ) ) ;
#11372 = DIRECTION ( 'NONE',  ( 0.9961255586397056438, 0.000000000000000000, -0.08794243244722427244 ) ) ;
#11373 = CARTESIAN_POINT ( 'NONE',  ( 2.651650429449553759, 13.87500000000000000, -0.8483495705504471296 ) ) ;
#11374 = CARTESIAN_POINT ( 'NONE',  ( -63.16055005427053004, 15.00000000000000000, -202.1988008120308677 ) ) ;
#11375 = CIRCLE ( 'NONE', #7666, 4.000000000000000000 ) ;
#11376 = CARTESIAN_POINT ( 'NONE',  ( -6.985256918799295889, 14.01682499433758444, -104.5239518528136529 ) ) ;
#11377 = AXIS2_PLACEMENT_3D ( 'NONE', #6441, #349, #5062 ) ;
#11378 = CARTESIAN_POINT ( 'NONE',  ( -2.298097038856278473, 11.12500000000000000, -1.201902961143720416 ) ) ;
#11379 = CIRCLE ( 'NONE', #520, 0.9999999999999731326 ) ;
#11380 = CARTESIAN_POINT ( 'NONE',  ( -8.842600465860288139, 2.075239479414269894, -40.10276331981361864 ) ) ;
#11381 = EDGE_CURVE ( 'NONE', #673, #10375, #8493, .T. ) ;
#11382 = CARTESIAN_POINT ( 'NONE',  ( -16.94138229547582242, 15.00000000000000000, -154.2864167784019003 ) ) ;
#11383 = CARTESIAN_POINT ( 'NONE',  ( 2.298097038856279362, 8.875000000000001776, -1.201902961143720860 ) ) ;
#11384 = CARTESIAN_POINT ( 'NONE',  ( -4.254413237569938389, 9.999999999999998224, -48.18981741835666810 ) ) ;
#11385 = CARTESIAN_POINT ( 'NONE',  ( -26.78870578381917866, 4.999999999999999112, -139.1599602021251769 ) ) ;
#11386 = EDGE_LOOP ( 'NONE', ( #4178, #10331 ) ) ;
#11387 = CARTESIAN_POINT ( 'NONE',  ( 8.949251933909494028, 11.66085798210991697, 2.227471517426460768 ) ) ;
#11388 = PLANE ( 'NONE',  #5740 ) ;
#11389 = CARTESIAN_POINT ( 'NONE',  ( 2.651650429449553314, 15.37500000000000178, -0.8483495705504476847 ) ) ;
#11390 = CARTESIAN_POINT ( 'NONE',  ( -1.346194077712558945, 13.56250000000000000, -0.2500000000000002220 ) ) ;
#11391 = CARTESIAN_POINT ( 'NONE',  ( 3.249999999999998224, 14.18750000000000178, -4.846194077712561388 ) ) ;
#11392 = ORIENTED_EDGE ( 'NONE', *, *, #12738, .T. ) ;
#11393 = VECTOR ( 'NONE', #11872, 1000.000000000000000 ) ;
#11394 = SHAPE_REPRESENTATION ( 'MAS-153', ( #1288, #5969, #9179, #14132, #11879, #15127, #5721, #9680, #12651 ), #55 ) ;
#11395 = CARTESIAN_POINT ( 'NONE',  ( 3.249999999999998668, 10.68750000000000000, -4.846194077712560500 ) ) ;
#11396 = DIRECTION ( 'NONE',  ( -0.000000000000000000, -1.000000000000000000, -0.000000000000000000 ) ) ;
#11397 = DIRECTION ( 'NONE',  ( 0.05964429961207439596, 0.000000000000000000, 0.9982196940171963462 ) ) ;
#11398 = CARTESIAN_POINT ( 'NONE',  ( -24.64653759749926465, 4.000000000000000000, -208.9889250379274301 ) ) ;
#11399 = DIRECTION ( 'NONE',  ( 0.9997619372588931741, 0.000000000000000000, 0.02181900108494707474 ) ) ;
#11400 = COORDINATED_UNIVERSAL_TIME_OFFSET ( 0, 0, .AHEAD. ) ;
#11401 = ADVANCED_FACE ( 'NONE', ( #9329 ), #13114, .T. ) ;
#11402 = CARTESIAN_POINT ( 'NONE',  ( 9.875992363362541937, 15.00000000000000000, -120.1725736632532318 ) ) ;
#11403 = DIRECTION ( 'NONE',  ( 0.000000000000000000, 0.000000000000000000, -1.000000000000000000 ) ) ;
#11404 = EDGE_CURVE ( 'NONE', #5270, #1429, #1062, .T. ) ;
#11405 = FACE_OUTER_BOUND ( 'NONE', #1328, .T. ) ;
#11406 = VERTEX_POINT ( 'NONE', #4685 ) ;
#11407 = CARTESIAN_POINT ( 'NONE',  ( 3.249999999999998668, 3.687500000000000444, -4.846194077712560500 ) ) ;
#11408 = CARTESIAN_POINT ( 'NONE',  ( -21.09070732192979492, 4.000000000000000000, -162.5659300234576676 ) ) ;
#11409 = CARTESIAN_POINT ( 'NONE',  ( -3.750000000000000000, 3.812500000000000888, -5.053300858899105741 ) ) ;
#11410 = EDGE_LOOP ( 'NONE', ( #3691, #13429, #14343, #5831 ) ) ;
#11411 = CARTESIAN_POINT ( 'NONE',  ( 6.079769598696780797, 1.750000000000736966, 52.20213348949025089 ) ) ;
#11412 = LINE ( 'NONE', #2863, #8735 ) ;
#11413 = APPROVAL_PERSON_ORGANIZATION ( #13046, #13137, #5706 ) ;
#11414 = CARTESIAN_POINT ( 'NONE',  ( -3.749999999999999556, 6.312500000000000888, -5.053300858899104853 ) ) ;
#11415 = CARTESIAN_POINT ( 'NONE',  ( -25.45939401113465550, 0.6794050853239335108, -205.0195236891385377 ) ) ;
#11416 = CARTESIAN_POINT ( 'NONE',  ( 3.194064371195536545, 3.228176745887314958, 4.887617669977396773 ) ) ;
#11417 = CARTESIAN_POINT ( 'NONE',  ( -1.553300858899107073, 3.437500000000000000, -7.250000000000000000 ) ) ;
#11418 = DATE_AND_TIME ( #9095, #565 ) ;
#11419 = LINE ( 'NONE', #7937, #13931 ) ;
#11420 = EDGE_CURVE ( 'NONE', #14600, #2663, #6926, .T. ) ;
#11421 = ORIENTED_EDGE ( 'NONE', *, *, #12628, .T. ) ;
#11422 = CARTESIAN_POINT ( 'NONE',  ( -2.298097038856278029, 1.625000000000000000, -1.201902961143720638 ) ) ;
#11423 = CARTESIAN_POINT ( 'NONE',  ( -2.802205527622656955, 9.999999999999996447, -108.2424688405072288 ) ) ;
#11424 = AXIS2_PLACEMENT_3D ( 'NONE', #1691, #5098, #9962 ) ;
#11425 = CARTESIAN_POINT ( 'NONE',  ( 1.553300858899109071, 7.437499999999999112, 0.2499999999999989175 ) ) ;
#11426 = CARTESIAN_POINT ( 'NONE',  ( 2.651650429449553759, 13.87500000000000000, -0.8483495705504471296 ) ) ;
#11427 = CARTESIAN_POINT ( 'NONE',  ( -9.347739544678665524, 4.300886386704505959, -115.3723878648253844 ) ) ;
#11428 = CARTESIAN_POINT ( 'NONE',  ( -9.525540565743067845, 3.627568584023658005, -116.4087343257889131 ) ) ;
#11429 = CARTESIAN_POINT ( 'NONE',  ( 3.249999999999998668, 8.687500000000000000, -4.846194077712560500 ) ) ;
#11430 = CARTESIAN_POINT ( 'NONE',  ( -3.249999999999999112, 0.6875000000000000000, -2.153805922287440833 ) ) ;
#11431 = CARTESIAN_POINT ( 'NONE',  ( -0.4453226528549816265, -2.225540348348185052E-17, 2.000000000000000000 ) ) ;
#11432 = PERSON_AND_ORGANIZATION_ROLE ( 'design_supplier' ) ;
#11433 = DIRECTION ( 'NONE',  ( 0.000000000000000000, 1.000000000000000000, 0.000000000000000000 ) ) ;
#11434 = VECTOR ( 'NONE', #14547, 1000.000000000000227 ) ;
#11435 = CARTESIAN_POINT ( 'NONE',  ( 13.78275167297412906, 6.000000000000000000, -126.2206732457524794 ) ) ;
#11436 = EDGE_LOOP ( 'NONE', ( #3360, #9310, #6523, #1048 ) ) ;
#11437 = CARTESIAN_POINT ( 'NONE',  ( -25.68866767343566693, 0.000000000000000000, -190.1221061183514962 ) ) ;
#11438 = CARTESIAN_POINT ( 'NONE',  ( -24.86990227130816322, 4.999999999999999112, -145.8847246090277281 ) ) ;
#11439 = CARTESIAN_POINT ( 'NONE',  ( -36.83003495301479546, 15.00000000000000000, -151.3633490263993053 ) ) ;
#11440 = CARTESIAN_POINT ( 'NONE',  ( 2.298097038856279362, 4.375000000000000888, -1.201902961143720860 ) ) ;
#11441 = ORIENTED_EDGE ( 'NONE', *, *, #5172, .T. ) ;
#11442 = CARTESIAN_POINT ( 'NONE',  ( 42.09231163430414568, 1.632027846204027168E-15, 51.87369981213807080 ) ) ;
#11443 = DIRECTION ( 'NONE',  ( 0.9961255586397056438, 0.000000000000000000, -0.08794243244722427244 ) ) ;
#11444 = CARTESIAN_POINT ( 'NONE',  ( 8.935898484867617952, 10.32733530284803436, 2.839335920898358623 ) ) ;
#11445 = CARTESIAN_POINT ( 'NONE',  ( -0.8896971555284219901, 1.636639605872992197E-12, -104.6801027822252053 ) ) ;
#11446 = VECTOR ( 'NONE', #12605, 1000.000000000000000 ) ;
#11447 = CARTESIAN_POINT ( 'NONE',  ( -3.249999999999999112, 11.81250000000000178, -4.846194077712558723 ) ) ;
#11448 = AXIS2_PLACEMENT_3D ( 'NONE', #2668, #5219, #14344 ) ;
#11449 = B_SPLINE_CURVE_WITH_KNOTS ( 'NONE', 3,
 ( #2565, #6107, #8579, #2876, #14400, #1473, #7576, #3955, #13313, #10820, #12139, #9668, #2798, #237, #2717, #3798, #8503, #13238, #2639, #7343, #12056, #11060, #8663, #5036, #1556, #14482, #7501, #12221, #1632, #477, #6347, #12370 ),
 .UNSPECIFIED., .F., .F.,
 ( 4, 2, 2, 2, 2, 2, 2, 2, 2, 2, 2, 2, 2, 2, 2, 4 ),
 ( 8.673617379884033931E-18, 0.004084815278923605887, 0.008169630557847203101, 0.01633926111569434375, 0.02042407639461791755, 0.02450889167354148787, 0.03267852223138869444, 0.04084815278923590448, 0.04289056042869772434, 0.04493296806815954419, 0.04901778334708325330, 0.05310259862600696934, 0.05718741390493067844, 0.06127222918385440142, 0.06331463682331625598, 0.06535704446277812441 ),
 .UNSPECIFIED. ) ;
#11450 = CARTESIAN_POINT ( 'NONE',  ( 22.05157068915105611, -2.335861096501437513E-12, -147.3126055969182460 ) ) ;
#11451 = CARTESIAN_POINT ( 'NONE',  ( -2.651650429449552870, 13.12500000000000000, -0.8483495705504462414 ) ) ;
#11452 = CARTESIAN_POINT ( 'NONE',  ( -1.528156170053301510, 7.379999999999995453, -45.73714083922575213 ) ) ;
#11453 = CARTESIAN_POINT ( 'NONE',  ( -6.470761321916836728, 14.36593687500089089, -104.2727818228492680 ) ) ;
#11454 = CARTESIAN_POINT ( 'NONE',  ( 0.000000000000000000, 11.00000000000000000, -0.2500000000000002220 ) ) ;
#11455 = CARTESIAN_POINT ( 'NONE',  ( -5.966056897915851032, 10.00000000000000355, -117.7917496622050066 ) ) ;
#11456 = DIRECTION ( 'NONE',  ( -0.000000000000000000, 1.000000000000000000, -0.000000000000000000 ) ) ;
#11457 = CARTESIAN_POINT ( 'NONE',  ( 3.249999999999998668, 6.687500000000000888, -4.846194077712560500 ) ) ;
#11458 = VECTOR ( 'NONE', #1885, 1000.000000000000000 ) ;
#11459 = CARTESIAN_POINT ( 'NONE',  ( 0.5805642473514114332, 5.000000000000000888, -138.6354391050098229 ) ) ;
#11460 = DIRECTION ( 'NONE',  ( 0.4975038378410474027, 0.000000000000000000, -0.8674617751425297563 ) ) ;
#11461 = EDGE_LOOP ( 'NONE', ( #11265, #2004, #999, #3592 ) ) ;
#11462 = ORIENTED_EDGE ( 'NONE', *, *, #2812, .T. ) ;
#11463 = CARTESIAN_POINT ( 'NONE',  ( -19.02652486928245068, 4.000000000000000000, -198.3523810112471040 ) ) ;
#11464 = CARTESIAN_POINT ( 'NONE',  ( 3.750000000000000000, 2.750000000000000000, -3.500000000000000444 ) ) ;
#11465 = CARTESIAN_POINT ( 'NONE',  ( 0.000000000000000000, 14.50000000000000355, -0.2500000000000002220 ) ) ;
#11466 = FACE_OUTER_BOUND ( 'NONE', #7431, .T. ) ;
#11467 = ORIENTED_EDGE ( 'NONE', *, *, #2714, .T. ) ;
#11468 = CARTESIAN_POINT ( 'NONE',  ( 2.298097038856279362, 11.87500000000000000, -1.201902961143720860 ) ) ;
#11469 = EDGE_CURVE ( 'NONE', #2776, #13242, #12966, .T. ) ;
#11470 = CIRCLE ( 'NONE', #4802, 2.000000000000001776 ) ;
#11471 = CARTESIAN_POINT ( 'NONE',  ( -3.054861441201806915, -2.473751543679003184, -1.000000000000011768 ) ) ;
#11472 = CARTESIAN_POINT ( 'NONE',  ( -1.346194077712559389, 7.437500000000000888, -6.749999999999999112 ) ) ;
#11473 = CARTESIAN_POINT ( 'NONE',  ( -8.621472139734160933, 11.69044914895178700, -105.3716763026984040 ) ) ;
#11474 = CARTESIAN_POINT ( 'NONE',  ( -7.369174163213084938, 14.17702046568131635, -116.5771123024624103 ) ) ;
#11475 = PERSON_AND_ORGANIZATION ( #8514, #11600 ) ;
#11476 = CARTESIAN_POINT ( 'NONE',  ( 9.667889503862193479, 15.00000000000093614, -108.9228968456952344 ) ) ;
#11477 = CARTESIAN_POINT ( 'NONE',  ( 5.844703153020811115, 15.00000000000000000, -103.2023327213425432 ) ) ;
#11478 = EDGE_LOOP ( 'NONE', ( #7226, #12140, #11159 ) ) ;
#11479 = CIRCLE ( 'NONE', #12718, 5.000000000000004441 ) ;
#11480 = CARTESIAN_POINT ( 'NONE',  ( 26.39556552446789794, 2.215704797542763949, -137.6676921094336876 ) ) ;
#11481 = CARTESIAN_POINT ( 'NONE',  ( 2.298097038856278473, 9.625000000000000000, -5.798097038856279362 ) ) ;
#11482 = B_SPLINE_CURVE_WITH_KNOTS ( 'NONE', 3,
 ( #12011, #9548, #2675, #7066, #10781, #123, #13194, #7218, #280, #11785, #1282, #13271, #7375, #12092, #5984, #198, #1516, #4994 ),
 .UNSPECIFIED., .F., .F.,
 ( 4, 2, 2, 2, 2, 2, 2, 2, 4 ),
 ( -1.076588104275207311E-05, 0.0002386119086020659368, 0.0004879896982468839568, 0.0009867452775365226532, 0.001984256436115799938, 0.002483012015405438363, 0.002981767594695076788, 0.003480523173984714780, 0.003979278753274353639 ),
 .UNSPECIFIED. ) ;
#11483 = VERTEX_POINT ( 'NONE', #10785 ) ;
#11484 = EDGE_LOOP ( 'NONE', ( #14508, #190, #2409, #7996 ) ) ;
#11485 = CARTESIAN_POINT ( 'NONE',  ( -3.980102097228897245E-16, 4.500000000000000888, -6.749999999999999112 ) ) ;
#11486 = CARTESIAN_POINT ( 'NONE',  ( -2.837468109123414628, -2.529993217055221510, -0.7946808062269109518 ) ) ;
#11487 =( BOUNDED_SURFACE ( )  B_SPLINE_SURFACE ( 3, 2, ( 
 ( #14173, #3646, #8349 ),
 ( #8278, #10377, #18 ),
 ( #4734, #2114, #3414 ),
 ( #6820, #3576, #6890 ),
 ( #951, #5656, #3343 ),
 ( #4654, #11610, #8202 ),
 ( #11827, #4507, #8124 ),
 ( #9215, #13006, #2266 ),
 ( #8051, #12779, #6971 ),
 ( #1029, #5735, #3962 ),
 ( #10911, #13399, #6276 ),
 ( #3804, #8668, #7507 ),
 ( #4041, #4960, #7185 ),
 ( #9675, #7349, #482 ),
 ( #9592, #3724, #2803 ),
 ( #10756, #8429, #14644 ),
 ( #2723, #13162, #12226 ),
 ( #12145, #14320, #1637 ),
 ( #6352, #1562, #6114 ),
 ( #13075, #5116, #13318 ) ),
 .UNSPECIFIED., .F., .F., .F. ) 
 B_SPLINE_SURFACE_WITH_KNOTS ( ( 4, 2, 2, 2, 2, 2, 2, 2, 2, 4 ),
 ( 3, 3 ),
 ( 0.04111226598309934699, 0.04870987420823701119, 0.05630748243337466846, 0.07150269888364998994, 0.07530150299621882204, 0.07910030710878765414, 0.08669791533392531835, 0.09429552355906298255, 0.09809432767163181466, 0.1018931317842006329 ),
 ( 0.000000000000000000, 0.8628733549542494385 ),
 .UNSPECIFIED. ) 
 GEOMETRIC_REPRESENTATION_ITEM ( )  RATIONAL_B_SPLINE_SURFACE ( (
 ( 1.000000000000000000, 0.7472702456390871717, 0.9306880333625028312),
 ( 1.000000000000000000, 0.7472702456390871717, 0.9306880333625028312),
 ( 1.000000000000000000, 0.7472702456390871717, 0.9306880333625028312),
 ( 1.000000000000000000, 0.7472702456390871717, 0.9306880333625028312),
 ( 1.000000000000000000, 0.7472702456390871717, 0.9306880333625028312),
 ( 1.000000000000000000, 0.7472702456390871717, 0.9306880333625028312),
 ( 1.000000000000000000, 0.7472702456390872827, 0.9306880333625028312),
 ( 1.000000000000000000, 0.7472702456390872827, 0.9306880333625028312),
 ( 1.000000000000000000, 0.7472702456390861725, 0.9306880333625024981),
 ( 1.000000000000000000, 0.7472702456390861725, 0.9306880333625024981),
 ( 1.000000000000000000, 0.7472702456390871717, 0.9306880333625028312),
 ( 1.000000000000000000, 0.7472702456390871717, 0.9306880333625028312),
 ( 1.000000000000000000, 0.7472702456390862835, 0.9306880333625024981),
 ( 1.000000000000000000, 0.7472702456390862835, 0.9306880333625024981),
 ( 1.000000000000000000, 0.7472702456390871717, 0.9306880333625028312),
 ( 1.000000000000000000, 0.7472702456390871717, 0.9306880333625028312),
 ( 1.000000000000000000, 0.7472702456390863945, 0.9306880333625026092),
 ( 1.000000000000000000, 0.7472702456390863945, 0.9306880333625026092),
 ( 1.000000000000000000, 0.7472702456390870607, 0.9306880333625027202),
 ( 1.000000000000000000, 0.7472702456390870607, 0.9306880333625027202) ) ) 
 REPRESENTATION_ITEM ( '' )  SURFACE ( )  );
#11488 = CARTESIAN_POINT ( 'NONE',  ( 1.553300858899109516, 2.437500000000000444, 0.2499999999999993616 ) ) ;
#11489 = ORIENTED_EDGE ( 'NONE', *, *, #534, .F. ) ;
#11490 = CYLINDRICAL_SURFACE ( 'NONE', #14412, 3.250000000000005329 ) ;
#11491 = CARTESIAN_POINT ( 'NONE',  ( 2.298097038856279362, 0.8750000000000000000, -1.201902961143720860 ) ) ;
#11492 = CARTESIAN_POINT ( 'NONE',  ( -1.553300858899107295, 4.437500000000000888, -7.250000000000000000 ) ) ;
#11493 = EDGE_CURVE ( 'NONE', #12677, #10395, #5840, .T. ) ;
#11494 = CARTESIAN_POINT ( 'NONE',  ( -25.25620482601053141, 6.788815924111790495E-10, -199.8982617752898818 ) ) ;
#11495 = PLANE ( 'NONE',  #1034 ) ;
#11496 = CALENDAR_DATE ( 2026, 8, 10 ) ;
#11497 = CARTESIAN_POINT ( 'NONE',  ( 9.381253443180193941, 5.000000000000000888, -119.0445822199432797 ) ) ;
#11498 = FACE_OUTER_BOUND ( 'NONE', #13803, .T. ) ;
#11499 = ORIENTED_EDGE ( 'NONE', *, *, #8561, .T. ) ;
#11500 = CARTESIAN_POINT ( 'NONE',  ( -2.298097038856278029, 5.625000000000000000, -1.201902961143720638 ) ) ;
#11501 = CYLINDRICAL_SURFACE ( 'NONE', #1552, 5.000000000000000888 ) ;
#11502 = EDGE_CURVE ( 'NONE', #3391, #12700, #7003, .T. ) ;
#11503 = CARTESIAN_POINT ( 'NONE',  ( 3.749999999999999556, 11.25000000000000178, -3.500000000000000444 ) ) ;
#11504 = EDGE_CURVE ( 'NONE', #9540, #3493, #10345, .T. ) ;
#11505 = CARTESIAN_POINT ( 'NONE',  ( 3.749999999999999112, 13.68750000000000000, -5.053300858899108405 ) ) ;
#11506 = EDGE_CURVE ( 'NONE', #973, #5826, #613, .T. ) ;
#11507 = CARTESIAN_POINT ( 'NONE',  ( -64.96178392459071915, 14.30069434053429589, -197.3172887038956844 ) ) ;
#11508 = DIRECTION ( 'NONE',  ( 0.000000000000000000, 0.000000000000000000, 1.000000000000000000 ) ) ;
#11509 = CARTESIAN_POINT ( 'NONE',  ( 0.000000000000000000, 0.5000000000000001110, -0.2500000000000002220 ) ) ;
#11510 = CARTESIAN_POINT ( 'NONE',  ( 11.18769411126905666, 13.31779969966692789, -106.3797690317953766 ) ) ;
#11511 = CARTESIAN_POINT ( 'NONE',  ( 2.162407246366561786, -2.421043869676734683, -85.55495855355363233 ) ) ;
#11512 = LINE ( 'NONE', #11435, #9497 ) ;
#11513 = ORIENTED_EDGE ( 'NONE', *, *, #6499, .F. ) ;
#11514 = CARTESIAN_POINT ( 'NONE',  ( -29.80626542450986349, 3.999999999999753975, -200.5060461161095020 ) ) ;
#11515 = DIRECTION ( 'NONE',  ( 0.000000000000000000, 1.000000000000000000, 0.000000000000000000 ) ) ;
#11516 = CARTESIAN_POINT ( 'NONE',  ( -7.279638199344828031, 0.04866399238529270366, -104.3603488955697571 ) ) ;
#11517 = CARTESIAN_POINT ( 'NONE',  ( 2.298097038856279362, 2.375000000000000000, -1.201902961143720860 ) ) ;
#11518 = ORIENTED_EDGE ( 'NONE', *, *, #11502, .T. ) ;
#11519 = CARTESIAN_POINT ( 'NONE',  ( -6.786583542010076187, 15.00000000000000000, -128.6396923774024401 ) ) ;
#11520 = CARTESIAN_POINT ( 'NONE',  ( -25.70420084062632426, 0.8205903998713498515, -205.0550399661483993 ) ) ;
#11521 = CARTESIAN_POINT ( 'NONE',  ( 8.887137379133079662, 12.34685406312035560, 5.073603994963653996 ) ) ;
#11522 = CARTESIAN_POINT ( 'NONE',  ( 0.2132689653687949716, 1.734723475976807094E-15, -112.6263465441575136 ) ) ;
#11523 = CARTESIAN_POINT ( 'NONE',  ( -3.980102097228897738E-16, 12.00000000000000178, -6.749999999999999112 ) ) ;
#11524 = FACE_OUTER_BOUND ( 'NONE', #11567, .T. ) ;
#11525 = CARTESIAN_POINT ( 'NONE',  ( -1.553300858899106629, 1.562500000000000222, 0.2500000000000002220 ) ) ;
#11526 = CARTESIAN_POINT ( 'NONE',  ( 3.230086961373100696, 9.999999999999998224, 5.208283729180108068 ) ) ;
#11527 = APPROVAL ( #14140, 'UNSPECIFIED' ) ;
#11528 = CARTESIAN_POINT ( 'NONE',  ( 4.286263797015736595E-16, 1.000000000000000000, 3.500000000000000000 ) ) ;
#11529 = CLOSED_SHELL ( 'NONE', ( #7699, #8655, #7678, #8755, #9513, #14914, #8057, #6563, #12152, #11186, #8833, #6783, #2436, #2912, #3567, #4516, #10077, #433, #7589, #5088, #5518 ) ) ;
#11530 = CYLINDRICAL_SURFACE ( 'NONE', #677, 16.00000000006737721 ) ;
#11531 = CARTESIAN_POINT ( 'NONE',  ( -7.366917200155316259, 2.099999999999999645, 17.31320944260497541 ) ) ;
#11532 = CARTESIAN_POINT ( 'NONE',  ( -1.346194077712559389, 10.06250000000000000, -0.2500000000000002220 ) ) ;
#11533 = CARTESIAN_POINT ( 'NONE',  ( 16.50094977371536231, 8.749999999999998224, -91.72275351520976017 ) ) ;
#11534 = CARTESIAN_POINT ( 'NONE',  ( -2.729969426660547871, 2.500000000000000000, -110.6850855677400602 ) ) ;
#11535 = ORIENTED_EDGE ( 'NONE', *, *, #7100, .T. ) ;
#11536 = ORIENTED_EDGE ( 'NONE', *, *, #438, .T. ) ;
#11537 = CARTESIAN_POINT ( 'NONE',  ( -1.553300858899106629, 1.062500000000000222, 0.2500000000000002220 ) ) ;
#11538 = CARTESIAN_POINT ( 'NONE',  ( -2.298097038856279362, 14.87500000000000355, -5.798097038856278473 ) ) ;
#11539 = CARTESIAN_POINT ( 'NONE',  ( 26.66376411343011910, 4.332989673203356595, -138.8074532758291468 ) ) ;
#11540 = ORIENTED_EDGE ( 'NONE', *, *, #4662, .T. ) ;
#11541 = CARTESIAN_POINT ( 'NONE',  ( -3.249999999999999112, 1.687499999999999778, -2.153805922287440833 ) ) ;
#11542 = CARTESIAN_POINT ( 'NONE',  ( -2.802205527622656955, 5.000000000000000888, -108.2424688405072430 ) ) ;
#11543 = CARTESIAN_POINT ( 'NONE',  ( -9.081120478662709772, 11.43401422448979687, -105.0943637814115164 ) ) ;
#11544 = CARTESIAN_POINT ( 'NONE',  ( 3.249999999999998668, 2.687500000000000888, -4.846194077712560500 ) ) ;
#11545 = COORDINATED_UNIVERSAL_TIME_OFFSET ( 0, 0, .AHEAD. ) ;
#11546 = CARTESIAN_POINT ( 'NONE',  ( 8.821381957849935063, 12.49999999999999822, -110.6350233298706485 ) ) ;
#11547 = CARTESIAN_POINT ( 'NONE',  ( 5.228075279701640099, 1.000000000000000000, -165.7939279834373849 ) ) ;
#11548 = EDGE_LOOP ( 'NONE', ( #841, #8424, #3802, #6909 ) ) ;
#11549 = CARTESIAN_POINT ( 'NONE',  ( 26.76147460282112789, 3.476039578919685624, -138.2546491778831239 ) ) ;
#11550 = CARTESIAN_POINT ( 'NONE',  ( -3.249999999999999556, 11.25000000000000000, -3.499999999999999556 ) ) ;
#11551 = EDGE_LOOP ( 'NONE', ( #13080, #4524, #14429 ) ) ;
#11552 = ORIENTED_EDGE ( 'NONE', *, *, #11115, .F. ) ;
#11553 = CARTESIAN_POINT ( 'NONE',  ( -2.651650429449553314, 9.875000000000000000, -6.151650429449552426 ) ) ;
#11554 = DIRECTION ( 'NONE',  ( 0.08794243244723003172, 0.000000000000000000, 0.9961255586397049777 ) ) ;
#11555 = CARTESIAN_POINT ( 'NONE',  ( -1.553300858899107073, -0.06249999999999988898, -7.249999999999999112 ) ) ;
#11556 = CARTESIAN_POINT ( 'NONE',  ( -3.249999999999999112, 5.687500000000000888, -2.153805922287440833 ) ) ;
#11557 = EDGE_LOOP ( 'NONE', ( #8507, #13926, #15165, #15189 ) ) ;
#11558 = CARTESIAN_POINT ( 'NONE',  ( 2.159942170319879562, 9.999999999999998224, -121.5147849362692369 ) ) ;
#11559 = CARTESIAN_POINT ( 'NONE',  ( 0.000000000000000000, 4.000000000000000000, -0.2500000000000002220 ) ) ;
#11560 = CARTESIAN_POINT ( 'NONE',  ( 0.000000000000000000, 4.000000000000000000, 0.2500000000000002220 ) ) ;
#11561 = CARTESIAN_POINT ( 'NONE',  ( -25.02281643586231752, 2.918594768585438537, -209.0154590114276232 ) ) ;
#11562 = CARTESIAN_POINT ( 'NONE',  ( -14.40544493037610430, 9.999999999999998224, -152.3816313692990434 ) ) ;
#11563 = DATE_TIME_ROLE ( 'creation_date' ) ;
#11564 = DIRECTION ( 'NONE',  ( -0.03706689162378395269, -0.5877852522924743583, 0.8081673977170961143 ) ) ;
#11565 = EDGE_CURVE ( 'NONE', #5152, #5770, #9248, .T. ) ;
#11566 = CYLINDRICAL_SURFACE ( 'NONE', #2097, 3.187847681061608540 ) ;
#11567 = EDGE_LOOP ( 'NONE', ( #11880, #13950, #10693, #6223 ) ) ;
#11568 = EDGE_CURVE ( 'NONE', #10459, #10124, #1521, .T. ) ;
#11569 = CARTESIAN_POINT ( 'NONE',  ( 2.298097038856278029, 9.125000000000001776, -5.798097038856279362 ) ) ;
#11570 = CARTESIAN_POINT ( 'NONE',  ( 11.04730217088347999, 12.66744776516167192, -107.1178495010082514 ) ) ;
#11571 = CARTESIAN_POINT ( 'NONE',  ( 1.553300858899105963, 9.062500000000003553, -7.249999999999999112 ) ) ;
#11572 = CARTESIAN_POINT ( 'NONE',  ( 2.651650429449552870, 12.62500000000000000, -6.151650429449554203 ) ) ;
#11573 = APPROVAL ( #5076, 'UNSPECIFIED' ) ;
#11574 = CARTESIAN_POINT ( 'NONE',  ( -65.20134947527711233, 14.82863921652322148, -191.2408552922258878 ) ) ;
#11575 = CARTESIAN_POINT ( 'NONE',  ( -3.566158703387691808, 0.1143801738294297626, -137.4717337110981248 ) ) ;
#11576 = CARTESIAN_POINT ( 'NONE',  ( -2.651650429449552870, 13.62500000000000000, -0.8483495705504463524 ) ) ;
#11577 = CARTESIAN_POINT ( 'NONE',  ( -6.708147162979256173, 4.336808689942017736E-16, -124.4601323014835401 ) ) ;
#11578 = CALENDAR_DATE ( 2026, 8, 10 ) ;
#11579 = DIRECTION ( 'NONE',  ( -0.3900731735287306656, 0.000000000000000000, -0.9207838613340399991 ) ) ;
#11580 = ORIENTED_EDGE ( 'NONE', *, *, #8954, .T. ) ;
#11581 = EDGE_CURVE ( 'NONE', #7480, #1063, #12196, .T. ) ;
#11582 = CARTESIAN_POINT ( 'NONE',  ( -28.31848045150696436, 3.999999999999600320, -204.6799762813750476 ) ) ;
#11583 = CARTESIAN_POINT ( 'NONE',  ( 2.298097038856279362, 3.875000000000000000, -1.201902961143720860 ) ) ;
#11584 = EDGE_CURVE ( 'NONE', #2594, #6618, #12770, .T. ) ;
#11585 = CARTESIAN_POINT ( 'NONE',  ( -60.74056104667560163, 14.99999999999732836, -188.2485173983686479 ) ) ;
#11586 = ADVANCED_FACE ( 'NONE', ( #5233 ), #8248, .T. ) ;
#11587 = CARTESIAN_POINT ( 'NONE',  ( -2.298097038856278029, 2.625000000000000000, -1.201902961143720638 ) ) ;
#11588 = VERTEX_POINT ( 'NONE', #14598 ) ;
#11589 = CARTESIAN_POINT ( 'NONE',  ( 3.136841903360911843, 9.999999999999998224, -104.4936450199714812 ) ) ;
#11590 = CARTESIAN_POINT ( 'NONE',  ( -25.28306627899824122, 0.01437449745307941250, -199.9124629347120106 ) ) ;
#11591 = CC_DESIGN_APPROVAL ( #15024, ( #2439 ) ) ;
#11592 = CARTESIAN_POINT ( 'NONE',  ( 5.612199600609121930, -5.296307347064899472E-31, -165.5340050431785528 ) ) ;
#11593 = CARTESIAN_POINT ( 'NONE',  ( 3.249999999999999556, 11.25000000000000178, -3.500000000000000000 ) ) ;
#11594 = VECTOR ( 'NONE', #8137, 1000.000000000000000 ) ;
#11595 = CARTESIAN_POINT ( 'NONE',  ( 20.84482309861272498, 5.000000000000000888, -149.6621754078162212 ) ) ;
#11596 = CARTESIAN_POINT ( 'NONE',  ( -1.553300858899106629, 0.5625000000000003331, 0.2500000000000002220 ) ) ;
#11597 = CARTESIAN_POINT ( 'NONE',  ( -0.3766621274091715987, -0.1687972351630583345, 0.1491815183709511161 ) ) ;
#11598 = CARTESIAN_POINT ( 'NONE',  ( 1.052436484934203831, 2.165641995257063801, -1.000000000000007772 ) ) ;
#11599 = CARTESIAN_POINT ( 'NONE',  ( -5.162848795631284737, 10.00000000000000178, -114.2525014220538822 ) ) ;
#11600 = ORGANIZATION ( 'NAUO-ORG5', 'UNSPECIFIED', 'UNSPECIFIED' ) ;
#11601 = CARTESIAN_POINT ( 'NONE',  ( -6.505077406322743450, 2.100000000000000089, 8.060717365551118618 ) ) ;
#11602 = CARTESIAN_POINT ( 'NONE',  ( 3.249999999999999112, 7.812500000000000000, -2.153805922287439945 ) ) ;
#11603 = AXIS2_PLACEMENT_3D ( 'NONE', #1897, #8848, #11246 ) ;
#11604 = ADVANCED_FACE ( 'NONE', ( #6147 ), #4792, .T. ) ;
#11605 = CARTESIAN_POINT ( 'NONE',  ( -25.82983890416511841, 15.00000000000000000, -142.4527639562402328 ) ) ;
#11606 = CARTESIAN_POINT ( 'NONE',  ( 9.044950117654433797, 0.000000000000000000, -141.4826476090360643 ) ) ;
#11607 = ORIENTED_EDGE ( 'NONE', *, *, #7064, .T. ) ;
#11608 = CC_DESIGN_DATE_AND_TIME_ASSIGNMENT ( #3526, #9253, ( #11099 ) ) ;
#11609 = ORIENTED_EDGE ( 'NONE', *, *, #13579, .F. ) ;
#11610 = CARTESIAN_POINT ( 'NONE',  ( -2.831701609851823065, 0.000000000000000000, -177.7686553741204136 ) ) ;
#11611 = CARTESIAN_POINT ( 'NONE',  ( -1.553300858899106629, 3.062500000000000000, 0.2500000000000002220 ) ) ;
#11612 = CARTESIAN_POINT ( 'NONE',  ( 0.000000000000000000, 0.4999999999999999445, 0.2499999999999998057 ) ) ;
#11613 = CARTESIAN_POINT ( 'NONE',  ( -0.2500000000000000555, 4.500000000000000888, -1.499999999999999778 ) ) ;
#11614 = ORIENTED_EDGE ( 'NONE', *, *, #11493, .T. ) ;
#11615 = CARTESIAN_POINT ( 'NONE',  ( 3.249999999999998224, 1.312500000000000000, -2.153805922287439945 ) ) ;
#11616 = TOROIDAL_SURFACE ( 'NONE', #12107, 4.000000000000001776, 1.000000000000000000 ) ;
#11617 = AXIS2_PLACEMENT_3D ( 'NONE', #4264, #13696, #10348 ) ;
#11618 = DIRECTION ( 'NONE',  ( 0.000000000000000000, -0.000000000000000000, 1.000000000000000000 ) ) ;
#11619 = VECTOR ( 'NONE', #14202, 1000.000000000000000 ) ;
#11620 = CARTESIAN_POINT ( 'NONE',  ( -8.429402173688821165, 12.15659329378483200, -105.2683602625900647 ) ) ;
#11621 = CARTESIAN_POINT ( 'NONE',  ( -3.980102097228897245E-16, 2.500000000000000000, -6.749999999999999112 ) ) ;
#11622 = CALENDAR_DATE ( 2026, 8, 10 ) ;
#11623 = FACE_OUTER_BOUND ( 'NONE', #9141, .T. ) ;
#11624 = CARTESIAN_POINT ( 'NONE',  ( -8.265142125449935762, 13.41314848964355022, -116.6996609440855650 ) ) ;
#11625 = ORIENTED_EDGE ( 'NONE', *, *, #12531, .T. ) ;
#11626 = CARTESIAN_POINT ( 'NONE',  ( -0.9215583806111760090, 14.99999999999999822, -108.4313125253715242 ) ) ;
#11627 = CARTESIAN_POINT ( 'NONE',  ( -2.298097038856278473, 12.12500000000000000, -1.201902961143720416 ) ) ;
#11628 = CIRCLE ( 'NONE', #4470, 1.000000000000000000 ) ;
#11629 = ORIENTED_EDGE ( 'NONE', *, *, #9798, .T. ) ;
#11630 = ORIENTED_EDGE ( 'NONE', *, *, #13747, .T. ) ;
#11631 = CARTESIAN_POINT ( 'NONE',  ( -1.553300858899106629, 10.56249999999999822, 0.2500000000000002220 ) ) ;
#11632 = DIRECTION ( 'NONE',  ( 0.000000000000000000, 0.000000000000000000, -1.000000000000000000 ) ) ;
#11633 = CARTESIAN_POINT ( 'NONE',  ( 2.651650429449554203, 5.375000000000000888, -0.8483495705504471296 ) ) ;
#11634 = CARTESIAN_POINT ( 'NONE',  ( -1.346194077712558945, 5.562500000000001776, -0.2500000000000002220 ) ) ;
#11635 = VERTEX_POINT ( 'NONE', #12019 ) ;
#11636 = CARTESIAN_POINT ( 'NONE',  ( -1.334601435092752419, 15.00000000000000000, -105.6792246796778869 ) ) ;
#11637 = CARTESIAN_POINT ( 'NONE',  ( -3.249999999999999556, 1.187500000000000444, -2.153805922287440833 ) ) ;
#11638 = B_SPLINE_SURFACE_WITH_KNOTS ( 'NONE', 1, 3, ( 
 ( #4439, #3421, #2123, #1115 ),
 ( #13954, #958, #10537, #2274 ) ),
 .UNSPECIFIED., .F., .F., .F.,
 ( 2, 2 ),
 ( 4, 4 ),
 ( 0.000000000000000000, 1.000000000000000000 ),
 ( 4.709001436419550934, 4.943672903615365932 ),
 .UNSPECIFIED. ) ;
#11639 = CARTESIAN_POINT ( 'NONE',  ( 3.249999999999998668, 11.68750000000000000, -4.846194077712560500 ) ) ;
#11640 = CARTESIAN_POINT ( 'NONE',  ( 2.651650429449553759, 5.875000000000000000, -0.8483495705504471296 ) ) ;
#11641 = AXIS2_PLACEMENT_3D ( 'NONE', #13434, #14595, #4150 ) ;
#11642 = CARTESIAN_POINT ( 'NONE',  ( -25.68188187296914293, 1.246347066919430979, -206.1291706975209763 ) ) ;
#11643 = CARTESIAN_POINT ( 'NONE',  ( -63.21422130130007133, 9.999999999999998224, -203.6040552426024703 ) ) ;
#11644 = COORDINATED_UNIVERSAL_TIME_OFFSET ( 0, 0, .AHEAD. ) ;
#11645 = CARTESIAN_POINT ( 'NONE',  ( -55.65458104879085255, 15.00000000000000178, -159.9470229874960694 ) ) ;
#11646 = ORIENTED_EDGE ( 'NONE', *, *, #10253, .F. ) ;
#11647 = CARTESIAN_POINT ( 'NONE',  ( -3.980102097228897738E-16, 5.999999999999999112, -6.749999999999999112 ) ) ;
#11648 = LOCAL_TIME ( 12, 28, 20.00000000000000000, #8552 ) ;
#11649 = CARTESIAN_POINT ( 'NONE',  ( -5.581362024073983186, 9.999999999999998224, -111.7646305296507165 ) ) ;
#11650 = CARTESIAN_POINT ( 'NONE',  ( 1.553300858899105963, 10.06250000000000000, -7.249999999999999112 ) ) ;
#11651 = CARTESIAN_POINT ( 'NONE',  ( 0.000000000000000000, 13.00000000000000178, 0.2500000000000002220 ) ) ;
#11652 = EDGE_CURVE ( 'NONE', #14341, #6054, #10864, .T. ) ;
#11653 = CARTESIAN_POINT ( 'NONE',  ( -64.98738446724354390, 14.92583229185657245, -188.2237117130508182 ) ) ;
#11654 = CARTESIAN_POINT ( 'NONE',  ( -0.2516503215200827648, -0.1858217187662949132, 0.1491815183709512271 ) ) ;
#11655 = CARTESIAN_POINT ( 'NONE',  ( -1.553300858899107073, 13.93750000000000000, -7.249999999999999112 ) ) ;
#11656 = DIRECTION ( 'NONE',  ( 0.000000000000000000, 1.000000000000000000, 0.000000000000000000 ) ) ;
#11657 = PERSON_AND_ORGANIZATION ( #3176, #3020 ) ;
#11658 = CC_DESIGN_APPROVAL ( #2516, ( #8454 ) ) ;
#11659 = CARTESIAN_POINT ( 'NONE',  ( 2.850044070969222076, 15.00000000000000000, -103.0233998225063345 ) ) ;
#11660 = ORIENTED_EDGE ( 'NONE', *, *, #4980, .T. ) ;
#11661 = CARTESIAN_POINT ( 'NONE',  ( -23.71521175673118975, 8.673617379884035472E-16, -202.9409338110467047 ) ) ;
#11662 = CARTESIAN_POINT ( 'NONE',  ( 3.249999999999998668, 4.687500000000000888, -4.846194077712560500 ) ) ;
#11663 = CIRCLE ( 'NONE', #4276, 0.2500000000000002220 ) ;
#11664 = CARTESIAN_POINT ( 'NONE',  ( -61.22190880152086123, 15.00000000000000000, -173.9954932429986059 ) ) ;
#11665 = CC_DESIGN_DATE_AND_TIME_ASSIGNMENT ( #11418, #7936, ( #8454 ) ) ;
#11666 = CARTESIAN_POINT ( 'NONE',  ( 3.249999999999998224, 1.187500000000000222, -4.846194077712561388 ) ) ;
#11667 = ORIENTED_EDGE ( 'NONE', *, *, #14054, .T. ) ;
#11668 = CARTESIAN_POINT ( 'NONE',  ( 4.921100845785776556, 9.999999999999996447, -108.2352075023247409 ) ) ;
#11669 = CARTESIAN_POINT ( 'NONE',  ( -0.2500000000000000555, 4.500000000000000888, -1.499999999999999778 ) ) ;
#11670 = CARTESIAN_POINT ( 'NONE',  ( 8.966408348210480383, 12.25254480171083671, 1.441352577737632590 ) ) ;
#11671 = CARTESIAN_POINT ( 'NONE',  ( -2.424117393066262061, 1.734723475976807094E-15, -107.6599666632789649 ) ) ;
#11672 = CARTESIAN_POINT ( 'NONE',  ( -3.249999999999999112, 13.81250000000000178, -4.846194077712558723 ) ) ;
#11673 = EDGE_CURVE ( 'NONE', #191, #10108, #2843, .T. ) ;
#11674 = CARTESIAN_POINT ( 'NONE',  ( 15.16156648836315490, 5.000000000000000888, -161.5519024490516529 ) ) ;
#11675 = CARTESIAN_POINT ( 'NONE',  ( 1.553300858899105963, 2.062500000000000000, -7.250000000000000888 ) ) ;
#11676 = AXIS2_PLACEMENT_3D ( 'NONE', #974, #5608, #12492 ) ;
#11677 = LINE ( 'NONE', #5867, #14427 ) ;
#11678 = EDGE_CURVE ( 'NONE', #11355, #15312, #14447, .T. ) ;
#11679 = CARTESIAN_POINT ( 'NONE',  ( -5.219328155730350360, 10.00000000000000178, -114.7721859121468810 ) ) ;
#11680 = FACE_OUTER_BOUND ( 'NONE', #11288, .T. ) ;
#11681 = CARTESIAN_POINT ( 'NONE',  ( -3.980102097228897245E-16, 13.50000000000000000, -6.749999999999999112 ) ) ;
#11682 = CARTESIAN_POINT ( 'NONE',  ( 2.538427055334838922, 15.00000000000006395, -24.40947673343477220 ) ) ;
#11683 = DIRECTION ( 'NONE',  ( 1.000000000000000000, 0.000000000000000000, 0.000000000000000000 ) ) ;
#11684 = ORIENTED_EDGE ( 'NONE', *, *, #5789, .T. ) ;
#11685 = ORIENTED_EDGE ( 'NONE', *, *, #3452, .F. ) ;
#11686 = CARTESIAN_POINT ( 'NONE',  ( -35.49029739244800652, 15.00000000000000000, -131.2404697308744517 ) ) ;
#11687 = CARTESIAN_POINT ( 'NONE',  ( 1.553300858899105963, 4.562500000000000888, -7.250000000000000888 ) ) ;
#11688 = VECTOR ( 'NONE', #2933, 1000.000000000000000 ) ;
#11689 = CARTESIAN_POINT ( 'NONE',  ( -1.553300858899107073, 2.937500000000000444, -7.249999999999999112 ) ) ;
#11690 = VECTOR ( 'NONE', #9414, 1000.000000000000114 ) ;
#11691 = CARTESIAN_POINT ( 'NONE',  ( 3.136841903360910067, 9.999999999999998224, -104.4936450199714812 ) ) ;
#11692 = VERTEX_POINT ( 'NONE', #443 ) ;
#11693 = CARTESIAN_POINT ( 'NONE',  ( 1.346194077712560944, 13.93750000000000000, -0.2500000000000010547 ) ) ;
#11694 = CARTESIAN_POINT ( 'NONE',  ( -48.84058141567145839, 15.00000000000000000, -150.0510139422299574 ) ) ;
#11695 = EDGE_CURVE ( 'NONE', #4145, #3581, #12457, .T. ) ;
#11696 = CARTESIAN_POINT ( 'NONE',  ( -8.489924801947323019, 12.60136528530092015, -104.4290565640461068 ) ) ;
#11697 = CARTESIAN_POINT ( 'NONE',  ( -2.298097038856278473, 5.125000000000000000, -1.201902961143720416 ) ) ;
#11698 = AXIS2_PLACEMENT_3D ( 'NONE', #4244, #5615, #12576 ) ;
#11699 = PERSON_AND_ORGANIZATION_ROLE ( 'classification_officer' ) ;
#11700 = LINE ( 'NONE', #8361, #3315 ) ;
#11701 = CARTESIAN_POINT ( 'NONE',  ( 10.27130088868191038, 1.514087034083648316E-12, -120.9123952260012089 ) ) ;
#11702 = ORIENTED_EDGE ( 'NONE', *, *, #8776, .T. ) ;
#11703 = CARTESIAN_POINT ( 'NONE',  ( 3.035840392568594837, -0.9800309627322405515, -1.000000000000001110 ) ) ;
#11704 = CARTESIAN_POINT ( 'NONE',  ( -1.346194077712559167, 12.43750000000000000, -6.749999999999999112 ) ) ;
#11705 = ORIENTED_EDGE ( 'NONE', *, *, #625, .T. ) ;
#11706 = VERTEX_POINT ( 'NONE', #3920 ) ;
#11707 = DIRECTION ( 'NONE',  ( -0.9997619372588931741, -0.000000000000000000, -0.02181900108494707474 ) ) ;
#11708 = CARTESIAN_POINT ( 'NONE',  ( 3.750000000000000000, 6.312500000000000000, -1.946699141100892705 ) ) ;
#11709 = CARTESIAN_POINT ( 'NONE',  ( -2.298097038856279362, 7.874999999999999112, -5.798097038856278473 ) ) ;
#11710 = ORIENTED_EDGE ( 'NONE', *, *, #3349, .F. ) ;
#11711 = CARTESIAN_POINT ( 'NONE',  ( -0.3214635616123167061, 9.999999999999998224, -103.0394908280460271 ) ) ;
#11712 = CARTESIAN_POINT ( 'NONE',  ( 2.298097038856279362, 3.875000000000000000, -1.201902961143720860 ) ) ;
#11713 = CARTESIAN_POINT ( 'NONE',  ( 1.553300858899105963, 9.562500000000000000, -7.250000000000000888 ) ) ;
#11714 = CARTESIAN_POINT ( 'NONE',  ( -24.96153981867218974, 3.396440209233427154, -209.3551883656818404 ) ) ;
#11715 = FACE_BOUND ( 'NONE', #7877, .T. ) ;
#11716 = LINE ( 'NONE', #13762, #12862 ) ;
#11717 = DATE_AND_TIME ( #4544, #10605 ) ;
#11718 = CARTESIAN_POINT ( 'NONE',  ( -52.04402637181858182, 15.00000000000000178, -154.2024637709381807 ) ) ;
#11719 = ORIENTED_EDGE ( 'NONE', *, *, #1110, .F. ) ;
#11720 = CARTESIAN_POINT ( 'NONE',  ( 3.249999999999999556, 7.250000000000000000, -3.500000000000000000 ) ) ;
#11721 = CARTESIAN_POINT ( 'NONE',  ( -10.29275726619092524, 0.000000000000000000, -34.56909192082969184 ) ) ;
#11722 = CARTESIAN_POINT ( 'NONE',  ( -3.750000000000000000, 9.812500000000000000, -5.053300858899105741 ) ) ;
#11723 = CARTESIAN_POINT ( 'NONE',  ( 3.749999999999999556, 11.81250000000000000, -1.946699141100892261 ) ) ;
#11724 = CARTESIAN_POINT ( 'NONE',  ( -63.60348060676461301, 15.00000000000000000, -180.2685449772604045 ) ) ;
#11725 = CARTESIAN_POINT ( 'NONE',  ( -7.195211678798691501, 5.000000000000000888, -124.1091578989210547 ) ) ;
#11726 = CARTESIAN_POINT ( 'NONE',  ( 2.651650429449554203, 12.37500000000000178, -0.8483495705504471296 ) ) ;
#11727 = CARTESIAN_POINT ( 'NONE',  ( -3.851617064430881143, 4.336808689942017243E-16, -107.8880831658969157 ) ) ;
#11728 = APPLICATION_PROTOCOL_DEFINITION ( 'international standard', 'config_control_design', 1994, #10340 ) ;
#11729 = DIRECTION ( 'NONE',  ( -0.000000000000000000, -1.000000000000000000, -0.000000000000000000 ) ) ;
#11730 = EDGE_LOOP ( 'NONE', ( #8717, #7837, #4673, #12276 ) ) ;
#11731 = CARTESIAN_POINT ( 'NONE',  ( 8.274725579668297470, 2.404323337855486908, 5.020935352624569248 ) ) ;
#11732 = CARTESIAN_POINT ( 'NONE',  ( -3.980102097228897245E-16, 3.500000000000000000, -6.749999999999999112 ) ) ;
#11733 = CARTESIAN_POINT ( 'NONE',  ( -63.02554947706173749, 15.00000000000000000, -201.1265914030478541 ) ) ;
#11734 = ADVANCED_FACE ( 'NONE', ( #3841 ), #14361, .T. ) ;
#11735 = CARTESIAN_POINT ( 'NONE',  ( -2.298097038856278029, 8.624999999999998224, -1.201902961143720638 ) ) ;
#11736 = ORIENTED_EDGE ( 'NONE', *, *, #12902, .T. ) ;
#11737 = CARTESIAN_POINT ( 'NONE',  ( -4.286587266701848975, 15.00000000000000000, -125.3643078127527133 ) ) ;
#11738 = CARTESIAN_POINT ( 'NONE',  ( 4.190455366039512519, 15.00000000000000000, -127.0204409346084873 ) ) ;
#11739 = CARTESIAN_POINT ( 'NONE',  ( 8.934261526981043033, 14.51811739220718422, 2.914342479709274958 ) ) ;
#11740 = CARTESIAN_POINT ( 'NONE',  ( -2.298097038856278473, 0.1250000000000000000, -1.201902961143720416 ) ) ;
#11741 = CARTESIAN_POINT ( 'NONE',  ( 2.298097038856278029, 14.12500000000000000, -5.798097038856279362 ) ) ;
#11742 = CARTESIAN_POINT ( 'NONE',  ( 1.624578347342658713, 8.673617379884035472E-16, -110.6108487083152454 ) ) ;
#11743 = CARTESIAN_POINT ( 'NONE',  ( 1.553300858899109516, 1.437500000000000000, 0.2499999999999993616 ) ) ;
#11744 = CARTESIAN_POINT ( 'NONE',  ( 7.148068729939690336, -2.490287375297125294, -34.56909192082981974 ) ) ;
#11745 = CARTESIAN_POINT ( 'NONE',  ( 84.71830840217509717, 4.000000000000000000, -172.4480499191751619 ) ) ;
#11746 = CARTESIAN_POINT ( 'NONE',  ( 0.3766621274091715987, -0.2500000000000000000, -7.146945437571387671 ) ) ;
#11747 = CARTESIAN_POINT ( 'NONE',  ( 12.01748009419283925, 0.000000000000000000, 57.58516622398010298 ) ) ;
#11748 = CARTESIAN_POINT ( 'NONE',  ( 3.249999999999998668, 12.68750000000000178, -4.846194077712560500 ) ) ;
#11749 = CARTESIAN_POINT ( 'NONE',  ( 3.869066569140437117, 14.96825566294793752, -13.02889994254487505 ) ) ;
#11750 = CARTESIAN_POINT ( 'NONE',  ( 3.235167919087375221, 8.673617379884035472E-16, -114.6791120453254962 ) ) ;
#11751 = ORIENTED_EDGE ( 'NONE', *, *, #3062, .F. ) ;
#11752 = PRODUCT_DEFINITION_SHAPE ( 'NONE', 'NONE',  #8454 ) ;
#11753 = ADVANCED_FACE ( 'NONE', ( #7379, #12096, #11173 ), #13438, .F. ) ;
#11754 = ORIENTED_EDGE ( 'NONE', *, *, #11967, .F. ) ;
#11755 = CARTESIAN_POINT ( 'NONE',  ( -6.038383049306157879, 2.646872844878069111E-13, -118.0543633388664659 ) ) ;
#11756 = CARTESIAN_POINT ( 'NONE',  ( 0.2499999999999999445, 5.000000000000000000, 1.500000000000000222 ) ) ;
#11757 = CARTESIAN_POINT ( 'NONE',  ( -3.749999999999999556, 6.312500000000000888, -5.053300858899104853 ) ) ;
#11758 = CARTESIAN_POINT ( 'NONE',  ( 1.553300858899105963, 3.062500000000000000, -7.249999999999999112 ) ) ;
#11759 = CARTESIAN_POINT ( 'NONE',  ( 7.353370788960563509, 9.999999999999998224, -111.8370434415688663 ) ) ;
#11760 = ORIENTED_EDGE ( 'NONE', *, *, #4385, .T. ) ;
#11761 = CARTESIAN_POINT ( 'NONE',  ( -1.346194077712559167, 1.937500000000000222, -6.749999999999999112 ) ) ;
#11762 = CARTESIAN_POINT ( 'NONE',  ( -4.122964195042672308, 5.000000000000000888, -110.0534507760547882 ) ) ;
#11763 = B_SPLINE_CURVE_WITH_KNOTS ( 'NONE', 3,
 ( #8054, #12782, #886, #8512, #12148, #3809, #1565, #2576, #8281, #1337 ),
 .UNSPECIFIED., .F., .F.,
 ( 4, 2, 2, 2, 4 ),
 ( 0.000000000000000000, 0.01417170859615501759, 0.02834341719231003517, 0.04251512578846505103, 0.05668683438462007035 ),
 .UNSPECIFIED. ) ;
#11764 = CARTESIAN_POINT ( 'NONE',  ( 18.09872976117486942, 8.673617379884035472E-16, -136.9430002941252269 ) ) ;
#11765 = CARTESIAN_POINT ( 'NONE',  ( 3.249999999999999556, 4.750000000000000000, -3.500000000000000000 ) ) ;
#11766 = DATE_AND_TIME ( #2277, #9389 ) ;
#11767 = CC_DESIGN_DATE_AND_TIME_ASSIGNMENT ( #12714, #12636, ( #4938 ) ) ;
#11768 = DIRECTION ( 'NONE',  ( 0.9989498407774362043, 0.000000000000000000, 0.04581719776170026931 ) ) ;
#11769 = CARTESIAN_POINT ( 'NONE',  ( 8.895820146902094550, 1.734723475976807094E-15, -117.6809082908677908 ) ) ;
#11770 = ORIENTED_EDGE ( 'NONE', *, *, #6874, .F. ) ;
#11771 = CARTESIAN_POINT ( 'NONE',  ( -2.570858214686514653, 15.00000000000000000, -122.5047453742639050 ) ) ;
#11772 = LINE ( 'NONE', #2587, #2755 ) ;
#11773 = ORIENTED_EDGE ( 'NONE', *, *, #10640, .F. ) ;
#11774 = EDGE_CURVE ( 'NONE', #6272, #6350, #14692, .T. ) ;
#11775 = ORIENTED_EDGE ( 'NONE', *, *, #1113, .F. ) ;
#11776 = CARTESIAN_POINT ( 'NONE',  ( 0.9523100111875538731, 2.331468351713773987E-16, 41.35525398876907133 ) ) ;
#11777 = CARTESIAN_POINT ( 'NONE',  ( 0.000000000000000000, 4.499999999999999112, 0.2500000000000002220 ) ) ;
#11778 = ADVANCED_FACE ( 'NONE', ( #14678 ), #5078, .T. ) ;
#11779 = CARTESIAN_POINT ( 'NONE',  ( -1.346194077712558945, 8.562500000000000000, -0.2500000000000002220 ) ) ;
#11781 = EDGE_CURVE ( 'NONE', #15055, #7289, #11700, .T. ) ;
#11780 = ORIENTED_EDGE ( 'NONE', *, *, #7971, .T. ) ;
#11782 = CARTESIAN_POINT ( 'NONE',  ( -0.5126277339646087006, 15.00000000000246203, -103.6859198938586815 ) ) ;
#11783 = CARTESIAN_POINT ( 'NONE',  ( -2.298097038856278918, 3.375000000000000000, -5.798097038856277585 ) ) ;
#11784 = CARTESIAN_POINT ( 'NONE',  ( 0.000000000000000000, 8.000000000000000000, 0.2500000000000002220 ) ) ;
#11785 = CARTESIAN_POINT ( 'NONE',  ( -8.590860326212494513, 0.8276621886826124319, -104.5228840682026288 ) ) ;
#11786 = DIRECTION ( 'NONE',  ( 1.000000000000000000, 0.000000000000000000, -0.000000000000000000 ) ) ;
#11787 = CARTESIAN_POINT ( 'NONE',  ( 6.049572344775472565, 15.00000000000000000, -111.4205638705285679 ) ) ;
#11788 = COORDINATED_UNIVERSAL_TIME_OFFSET ( 0, 0, .AHEAD. ) ;
#11789 = CARTESIAN_POINT ( 'NONE',  ( 2.548347919319509103, 1.829703814864835465, -1.000000000000001110 ) ) ;
#11790 = ORIENTED_EDGE ( 'NONE', *, *, #12707, .T. ) ;
#11791 = B_SPLINE_CURVE_WITH_KNOTS ( 'NONE', 3,
 ( #2611, #13448, #11035, #6153, #14371, #2852 ),
 .UNSPECIFIED., .F., .F.,
 ( 4, 2, 4 ),
 ( 0.000000000000000000, 0.0004983545201280861151, 0.0009967090402561722302 ),
 .UNSPECIFIED. ) ;
#11792 = CARTESIAN_POINT ( 'NONE',  ( 7.148068729939690336, 2.490287375297125294, -34.56909192082981974 ) ) ;
#11793 = CARTESIAN_POINT ( 'NONE',  ( -3.750000000000000000, 12.68750000000000178, -1.946699141100893149 ) ) ;
#11794 = CARTESIAN_POINT ( 'NONE',  ( 1.077968782234968836, 4.793811891163896277, -139.4304863127936471 ) ) ;
#11795 = CARTESIAN_POINT ( 'NONE',  ( -65.98103202930056455, 15.04542651531272490, -200.4630988027190881 ) ) ;
#11796 = CARTESIAN_POINT ( 'NONE',  ( -4.507264730511037598, -1.628626824712336107, -1.000000000000001332 ) ) ;
#11797 = CARTESIAN_POINT ( 'NONE',  ( 1.346194077712561166, 2.437500000000000444, -0.2500000000000011102 ) ) ;
#11798 = CARTESIAN_POINT ( 'NONE',  ( 9.390800893974766694, 1.188659780534533139, -106.3264951435503036 ) ) ;
#11799 = PERSON_AND_ORGANIZATION ( #3176, #3020 ) ;
#11800 = CYLINDRICAL_SURFACE ( 'NONE', #9971, 3.500000000000003109 ) ;
#11801 = CARTESIAN_POINT ( 'NONE',  ( 1.004809442601927394, 5.000000000000000888, -139.4752805618705622 ) ) ;
#11802 = VERTEX_POINT ( 'NONE', #2506 ) ;
#11803 = CARTESIAN_POINT ( 'NONE',  ( 8.840216610704089817, 3.990476221256948453, 2.799461104694893621 ) ) ;
#11804 = CARTESIAN_POINT ( 'NONE',  ( 3.249999999999999112, 1.812500000000000000, -2.153805922287439945 ) ) ;
#11805 = AXIS2_PLACEMENT_3D ( 'NONE', #1397, #9514, #2480 ) ;
#11806 = CARTESIAN_POINT ( 'NONE',  ( -65.59210620920288193, 15.00000000000000000, -187.0384419517383776 ) ) ;
#11807 = CARTESIAN_POINT ( 'NONE',  ( 2.298097038856278029, 5.125000000000000888, -5.798097038856279362 ) ) ;
#11808 = ORIENTED_EDGE ( 'NONE', *, *, #12628, .F. ) ;
#11809 = CARTESIAN_POINT ( 'NONE',  ( -5.574230463462276575, 9.999999999999998224, -116.5593450232789223 ) ) ;
#11810 = CARTESIAN_POINT ( 'NONE',  ( -1.500000000000000000, 5.000000000000000000, -0.2499999999999997780 ) ) ;
#11811 = CARTESIAN_POINT ( 'NONE',  ( -7.136800800203102035, 15.00000000000000000, -146.1984219328402048 ) ) ;
#11812 = CARTESIAN_POINT ( 'NONE',  ( -0.3766621274091713767, 0.2975415354274087432, -7.146945437571386783 ) ) ;
#11813 = CARTESIAN_POINT ( 'NONE',  ( 2.651650429449553314, 3.375000000000000444, -0.8483495705504476847 ) ) ;
#11814 = CARTESIAN_POINT ( 'NONE',  ( 3.749999999999999556, 4.812500000000000888, -1.946699141100892261 ) ) ;
#11815 = FACE_OUTER_BOUND ( 'NONE', #12262, .T. ) ;
#11816 = CARTESIAN_POINT ( 'NONE',  ( -1.553300858899107073, 3.937500000000001332, -7.249999999999999112 ) ) ;
#11817 = CARTESIAN_POINT ( 'NONE',  ( -13.68460728451510633, 7.499999999999991118, -92.46488696946715891 ) ) ;
#11818 = CARTESIAN_POINT ( 'NONE',  ( 9.068716941525979180, 1.734723475976807094E-15, -163.1923081219560174 ) ) ;
#11819 = CARTESIAN_POINT ( 'NONE',  ( -6.972928664498794227, 1.021521734388686209E-15, -104.3013574265779795 ) ) ;
#11820 = CARTESIAN_POINT ( 'NONE',  ( 26.04203104729493390, 0.000000000000000000, 69.41411580402545667 ) ) ;
#11821 = CARTESIAN_POINT ( 'NONE',  ( -1.346194077712559389, 12.43750000000000000, -6.749999999999999112 ) ) ;
#11822 = CARTESIAN_POINT ( 'NONE',  ( 1.855481649321456983, 15.00000000000000000, -35.83830032691798806 ) ) ;
#11823 = ORIENTED_EDGE ( 'NONE', *, *, #6650, .F. ) ;
#11824 = PRODUCT_DEFINITION_FORMATION_WITH_SPECIFIED_SOURCE ( 'ANY', '', #4992, .NOT_KNOWN. ) ;
#11825 = ORIENTED_EDGE ( 'NONE', *, *, #4891, .F. ) ;
#11826 = CARTESIAN_POINT ( 'NONE',  ( -5.248276757777016854, 1.059334121087498154E-12, -115.0315526420590118 ) ) ;
#11827 = CARTESIAN_POINT ( 'NONE',  ( -9.251449178678159413, 1.734723475976807094E-15, -178.3019022727991398 ) ) ;
#11828 = CARTESIAN_POINT ( 'NONE',  ( -2.651650429449552870, 3.125000000000000000, -0.8483495705504462414 ) ) ;
#11829 = CARTESIAN_POINT ( 'NONE',  ( 2.651650429449552870, 5.125000000000000000, -6.151650429449553314 ) ) ;
#11830 = VECTOR ( 'NONE', #5432, 1000.000000000000000 ) ;
#11831 = DIRECTION ( 'NONE',  ( 0.000000000000000000, 0.000000000000000000, -1.000000000000000000 ) ) ;
#11832 = VERTEX_POINT ( 'NONE', #33 ) ;
#11833 = CARTESIAN_POINT ( 'NONE',  ( -2.298097038856278029, 0.6249999999999998890, -1.201902961143720638 ) ) ;
#11834 = ADVANCED_FACE ( 'NONE', ( #11623 ), #1118, .F. ) ;
#11835 = CARTESIAN_POINT ( 'NONE',  ( 109.7555300068681419, 0.000000000000000000, 36.44134644672088541 ) ) ;
#11836 = APPROVAL_PERSON_ORGANIZATION ( #6982, #548, #3354 ) ;
#11837 = LINE ( 'NONE', #7358, #3213 ) ;
#11838 = EDGE_CURVE ( 'NONE', #13643, #2207, #5535, .T. ) ;
#11839 = CARTESIAN_POINT ( 'NONE',  ( -1.346194077712559389, 3.062500000000000000, -0.2500000000000002220 ) ) ;
#11840 = AXIS2_PLACEMENT_3D ( 'NONE', #12769, #14957, #4419 ) ;
#11841 = CARTESIAN_POINT ( 'NONE',  ( 16.30648644992872676, 8.673617379884035472E-16, -135.4745789036516612 ) ) ;
#11842 = ORIENTED_EDGE ( 'NONE', *, *, #801, .T. ) ;
#11843 = CARTESIAN_POINT ( 'NONE',  ( 5.000000000000000888, 9.999999999999998224, -108.9020125831789727 ) ) ;
#11844 = CARTESIAN_POINT ( 'NONE',  ( -2.298097038856278473, 13.12500000000000000, -1.201902961143720416 ) ) ;
#11845 = VERTEX_POINT ( 'NONE', #8291 ) ;
#11846 = ORIENTED_EDGE ( 'NONE', *, *, #1019, .F. ) ;
#11847 = DIRECTION ( 'NONE',  ( -0.3244857880293323671, -0.8090169943749464521, 0.4901025159897783312 ) ) ;
#11848 = CARTESIAN_POINT ( 'NONE',  ( 1.553300858899105963, 6.062500000000000888, -7.250000000000000888 ) ) ;
#11849 = CARTESIAN_POINT ( 'NONE',  ( 3.249999999999999556, 6.250000000000000888, -3.500000000000000000 ) ) ;
#11850 = EDGE_LOOP ( 'NONE', ( #11018, #5383, #3881, #4653 ) ) ;
#11851 = AXIS2_PLACEMENT_3D ( 'NONE', #13604, #617, #2929 ) ;
#11852 = CARTESIAN_POINT ( 'NONE',  ( -0.8896971555268431420, 14.99999999999876898, -104.6801027822232157 ) ) ;
#11853 = CIRCLE ( 'NONE', #276, 3.500000000000000000 ) ;
#11854 = CARTESIAN_POINT ( 'NONE',  ( 2.298097038856279362, 2.875000000000000000, -1.201902961143720860 ) ) ;
#11855 = VECTOR ( 'NONE', #3125, 1000.000000000000114 ) ;
#11856 = VECTOR ( 'NONE', #8252, 1000.000000000000000 ) ;
#11857 = CARTESIAN_POINT ( 'NONE',  ( -24.93348466747179870, 3.665517550122363577, -209.5032877194438470 ) ) ;
#11858 = CARTESIAN_POINT ( 'NONE',  ( 10.00452473099216988, 0.1207859802015546630, -163.8779166317577278 ) ) ;
#11859 = EDGE_CURVE ( 'NONE', #2651, #13498, #1846, .T. ) ;
#11860 = CARTESIAN_POINT ( 'NONE',  ( -0.2500000000000000555, 4.500000000000000888, 1.500000000000000222 ) ) ;
#11861 = APPLICATION_PROTOCOL_DEFINITION ( 'international standard', 'config_control_design', 1994, #5610 ) ;
#11862 = VECTOR ( 'NONE', #8023, 1000.000000000000000 ) ;
#11863 = CARTESIAN_POINT ( 'NONE',  ( 3.158384440324536691, 0.000000000000000000, -1.000000000000001332 ) ) ;
#11864 = VECTOR ( 'NONE', #1350, 1000.000000000000000 ) ;
#11865 = EDGE_LOOP ( 'NONE', ( #8049, #8672 ) ) ;
#11866 = CARTESIAN_POINT ( 'NONE',  ( -1.639428572435056353, 14.99999999999999822, -124.2686519725904333 ) ) ;
#11867 =( GEOMETRIC_REPRESENTATION_CONTEXT ( 3 ) GLOBAL_UNCERTAINTY_ASSIGNED_CONTEXT ( ( #8330 ) ) GLOBAL_UNIT_ASSIGNED_CONTEXT ( ( #2275, #13879, #6760 ) ) REPRESENTATION_CONTEXT ( 'NONE', 'WORKASPACE' ) );
#11869 = CARTESIAN_POINT ( 'NONE',  ( 1.553300858899109071, 11.43750000000000178, 0.2499999999999989175 ) ) ;
#11868 =( BOUNDED_SURFACE ( )  B_SPLINE_SURFACE ( 3, 1, ( 
 ( #9064, #3184 ),
 ( #1809, #10074 ),
 ( #13563, #7974 ),
 ( #13640, #2964 ) ),
 .UNSPECIFIED., .F., .F., .T. ) 
 B_SPLINE_SURFACE_WITH_KNOTS ( ( 4, 4 ),
 ( 2, 2 ),
 ( 0.000000000000000000, 1.000000000000000000 ),
 ( 0.000000000000000000, 1.000000000000000000 ),
 .UNSPECIFIED. ) 
 GEOMETRIC_REPRESENTATION_ITEM ( )  RATIONAL_B_SPLINE_SURFACE ( (
 ( 1.000000000000000000, 1.000000000000000000),
 ( 0.9719843790119068183, 0.9719843790119068183),
 ( 0.9719843790119068183, 0.9719843790119068183),
 ( 1.000000000000000000, 1.000000000000000000) ) ) 
 REPRESENTATION_ITEM ( '' )  SURFACE ( )  );
#11870 = CARTESIAN_POINT ( 'NONE',  ( -0.2500000000000000555, 4.500000000000000888, 1.500000000000000222 ) ) ;
#11871 = CARTESIAN_POINT ( 'NONE',  ( -64.10403461688579796, 13.26028305253761808, -210.3464984387109951 ) ) ;
#11872 = DIRECTION ( 'NONE',  ( -0.000000000000000000, -1.000000000000000000, -0.000000000000000000 ) ) ;
#11873 = CARTESIAN_POINT ( 'NONE',  ( 3.249999999999998224, 2.187500000000000000, -4.846194077712561388 ) ) ;
#11874 = CARTESIAN_POINT ( 'NONE',  ( 9.149651848773698859, 0.9864195427603029698, -106.2170607917651211 ) ) ;
#11875 = ADVANCED_FACE ( 'NONE', ( #4522 ), #5669, .F. ) ;
#11876 = APPROVAL_DATE_TIME ( #12901, #2654 ) ;
#11877 = CARTESIAN_POINT ( 'NONE',  ( -31.09209721305613527, 5.000000000000000888, -156.3611406121567597 ) ) ;
#11878 = DIRECTION ( 'NONE',  ( 0.05964429961207439596, -0.000000000000000000, 0.9982196940171963462 ) ) ;
#11879 = AXIS2_PLACEMENT_3D ( 'NONE', #13017, #7517, #12668 ) ;
#11880 = ORIENTED_EDGE ( 'NONE', *, *, #6545, .T. ) ;
#11881 = CARTESIAN_POINT ( 'NONE',  ( 5.705671018141757145, 2.650800484686449909, 4.619709739133793569 ) ) ;
#11882 = CARTESIAN_POINT ( 'NONE',  ( 2.298097038856278473, 3.625000000000000000, -5.798097038856279362 ) ) ;
#11883 = CARTESIAN_POINT ( 'NONE',  ( -8.195698801737231420, 0.4580377701651440203, -104.4390439392078918 ) ) ;
#11884 = CARTESIAN_POINT ( 'NONE',  ( 1.346194077712561166, 7.437500000000000000, -0.2500000000000011102 ) ) ;
#11885 = VERTEX_POINT ( 'NONE', #4667 ) ;
#11886 = CARTESIAN_POINT ( 'NONE',  ( -5.418245839020988441, 9.999999999999998224, -110.8346421744379313 ) ) ;
#11887 = CARTESIAN_POINT ( 'NONE',  ( 37.32986759126112730, 1.750000000000000000, 43.04214087805580391 ) ) ;
#11888 = CARTESIAN_POINT ( 'NONE',  ( -0.3498759111130647081, 9.999999999999998224, -139.6126861213997472 ) ) ;
#11889 = CARTESIAN_POINT ( 'NONE',  ( 3.249999999999999112, 0.8125000000000001110, -2.153805922287439945 ) ) ;
#11890 = CARTESIAN_POINT ( 'NONE',  ( 1.553300858899109071, 1.437500000000000000, 0.2499999999999989175 ) ) ;
#11891 = CARTESIAN_POINT ( 'NONE',  ( -1.553300858899107073, 5.437500000000001776, -7.250000000000000000 ) ) ;
#11892 = APPROVAL_PERSON_ORGANIZATION ( #9400, #4078, #8084 ) ;
#11893 = CARTESIAN_POINT ( 'NONE',  ( 2.860422134859789800, 8.673617379884037444E-16, -108.4900984580837644 ) ) ;
#11894 = CARTESIAN_POINT ( 'NONE',  ( -2.651650429449553314, 6.875000000000000000, -6.151650429449552426 ) ) ;
#11895 = CARTESIAN_POINT ( 'NONE',  ( 3.330118040168945637, 11.25215624712264173, 5.031695831575111022 ) ) ;
#11896 = CARTESIAN_POINT ( 'NONE',  ( -3.803913621930688382, 10.81208548464482355, -43.82788280992028263 ) ) ;
#11897 = TOROIDAL_SURFACE ( 'NONE', #10470, 4.000000000000000000, 1.000000000000000000 ) ;
#11898 = CARTESIAN_POINT ( 'NONE',  ( -9.721966606378851239, 15.00000000000000000, -116.3614657639809309 ) ) ;
#11899 = CARTESIAN_POINT ( 'NONE',  ( 2.298097038856279362, 10.87500000000000178, -1.201902961143720860 ) ) ;
#11900 = CARTESIAN_POINT ( 'NONE',  ( -12.74549125309000885, 3.999999999999993783, -151.2947804600756001 ) ) ;
#11901 = CARTESIAN_POINT ( 'NONE',  ( 3.249999999999998668, 11.68750000000000000, -4.846194077712560500 ) ) ;
#11902 = FACE_OUTER_BOUND ( 'NONE', #12265, .T. ) ;
#11903 = CARTESIAN_POINT ( 'NONE',  ( -63.72793358483406934, 15.00000000000018119, -180.7898741481596403 ) ) ;
#11904 = VERTEX_POINT ( 'NONE', #10393 ) ;
#11905 = CARTESIAN_POINT ( 'NONE',  ( 1.553300858899105963, 8.062500000000001776, -7.250000000000000888 ) ) ;
#11906 = ORIENTED_EDGE ( 'NONE', *, *, #3077, .T. ) ;
#11907 = CARTESIAN_POINT ( 'NONE',  ( -4.083223113469290233, 4.336808689942017736E-16, -107.4404827980595769 ) ) ;
#11908 = CARTESIAN_POINT ( 'NONE',  ( -0.8336906130587268260, -1.921202954650397032, -45.08225561976305329 ) ) ;
#11909 = CARTESIAN_POINT ( 'NONE',  ( -3.750000000000000000, 5.250000000000000000, -3.499999999999999112 ) ) ;
#11910 = CARTESIAN_POINT ( 'NONE',  ( 1.553300858899109071, 4.437499999999999112, 0.2499999999999989175 ) ) ;
#11911 = CYLINDRICAL_SURFACE ( 'NONE', #2558, 7.428243039713066764 ) ;
#11912 = ORIENTED_EDGE ( 'NONE', *, *, #8436, .F. ) ;
#11913 = TOROIDAL_SURFACE ( 'NONE', #15153, 1.250000000000002220, 1.750000000000000000 ) ;
#11914 = CARTESIAN_POINT ( 'NONE',  ( 3.249999999999998224, 6.187500000000001776, -4.846194077712561388 ) ) ;
#11915 = CARTESIAN_POINT ( 'NONE',  ( -68.83694965406208155, 9.999999999999998224, -180.7144811897190948 ) ) ;
#11916 = CARTESIAN_POINT ( 'NONE',  ( -3.756350458250083957, 9.999999999999998224, -48.23378863458027155 ) ) ;
#11917 = CARTESIAN_POINT ( 'NONE',  ( -2.298097038856278918, 6.375000000000000888, -5.798097038856277585 ) ) ;
#11918 =( REPRESENTATION_RELATIONSHIP ('NONE','NONE', #11394, #12380 ) REPRESENTATION_RELATIONSHIP_WITH_TRANSFORMATION ( #14824 )SHAPE_REPRESENTATION_RELATIONSHIP( ) );
#11919 = ITEM_DEFINED_TRANSFORMATION ( 'NONE', 'NONE', #9680,  #9419 ) ;
#11920 = DIRECTION ( 'NONE',  ( 0.000000000000000000, 0.000000000000000000, 1.000000000000000000 ) ) ;
#11921 = CARTESIAN_POINT ( 'NONE',  ( 26.93149290009008823, 8.673617379884035472E-16, -137.0203993314533761 ) ) ;
#11922 = ORIENTED_EDGE ( 'NONE', *, *, #14541, .F. ) ;
#11923 = AXIS2_PLACEMENT_3D ( 'NONE', #13684, #5253, #3081 ) ;
#11924 = PLANE ( 'NONE',  #12859 ) ;
#11925 = CARTESIAN_POINT ( 'NONE',  ( 0.000000000000000000, 4.000000000000000000, 0.000000000000000000 ) ) ;
#11926 = ORIENTED_EDGE ( 'NONE', *, *, #3195, .T. ) ;
#11927 = EDGE_CURVE ( 'NONE', #8744, #6645, #853, .T. ) ;
#11928 = ORIENTED_EDGE ( 'NONE', *, *, #13593, .F. ) ;
#11929 = CARTESIAN_POINT ( 'NONE',  ( -29.51225541722604007, 4.000000000000000888, -201.5661097356285723 ) ) ;
#11930 = CARTESIAN_POINT ( 'NONE',  ( -3.749999999999999556, 6.750000000000001776, -3.499999999999999112 ) ) ;
#11931 = CARTESIAN_POINT ( 'NONE',  ( -1.346194077712558945, 12.56250000000000355, -0.2500000000000002220 ) ) ;
#11932 = ORIENTED_EDGE ( 'NONE', *, *, #3922, .T. ) ;
#11933 = ADVANCED_FACE ( 'NONE', ( #9232, #3355 ), #3509, .F. ) ;
#11934 = CARTESIAN_POINT ( 'NONE',  ( 6.409599520805702610, 14.96732179972273435, 0.9270135685219680344 ) ) ;
#11935 = CARTESIAN_POINT ( 'NONE',  ( 3.249999999999999556, 8.750000000000000000, -3.500000000000000000 ) ) ;
#11936 = CIRCLE ( 'NONE', #4311, 0.2500000000000002220 ) ;
#11937 = AXIS2_PLACEMENT_3D ( 'NONE', #14795, #6577, #481 ) ;
#11938 = CARTESIAN_POINT ( 'NONE',  ( -8.934675013019075962, 2.500000000000000444, -123.2708221453725201 ) ) ;
#11939 = CARTESIAN_POINT ( 'NONE',  ( -53.54684834582479169, 10.00000000000000355, -170.1666570554936868 ) ) ;
#11940 = CARTESIAN_POINT ( 'NONE',  ( -50.40552334055468009, 15.00000000000000000, -158.2257257439712532 ) ) ;
#11941 = COORDINATED_UNIVERSAL_TIME_OFFSET ( 0, 0, .AHEAD. ) ;
#11942 = DIRECTION ( 'NONE',  ( -0.8645818496218652394, 0.000000000000000000, 0.5024920151648527566 ) ) ;
#11943 = ORIENTED_EDGE ( 'NONE', *, *, #10342, .T. ) ;
#11944 = AXIS2_PLACEMENT_3D ( 'NONE', #14107, #10541, #10471 ) ;
#11945 = ADVANCED_FACE ( 'NONE', ( #8215 ), #10484, .T. ) ;
#11946 = CARTESIAN_POINT ( 'NONE',  ( 2.651650429449553314, 12.37500000000000178, -0.8483495705504476847 ) ) ;
#11947 = CARTESIAN_POINT ( 'NONE',  ( 1.077968782234507428, 5.000000000000000888, -139.4304863127929082 ) ) ;
#11948 = CARTESIAN_POINT ( 'NONE',  ( -67.58441209323089538, 10.23658426854694170, -204.5076973825927666 ) ) ;
#11949 = CARTESIAN_POINT ( 'NONE',  ( 5.000000000000000000, 5.000000000000000888, -1.663700395152567513 ) ) ;
#11950 = CARTESIAN_POINT ( 'NONE',  ( -2.298097038856279362, 3.875000000000000444, -5.798097038856278473 ) ) ;
#11951 = VECTOR ( 'NONE', #5034, 1000.000000000000000 ) ;
#11952 = CARTESIAN_POINT ( 'NONE',  ( 8.755026559824571564, 0.6305609032749204257, -105.6652816485397040 ) ) ;
#11953 = DATE_AND_TIME ( #14613, #11648 ) ;
#11954 = CARTESIAN_POINT ( 'NONE',  ( -4.030963197337185555, 14.27759960331617428, -125.2321359900997209 ) ) ;
#11955 = CARTESIAN_POINT ( 'NONE',  ( -25.68053481550299111, 5.000000000000000888, -142.4798935003980773 ) ) ;
#11956 = CC_DESIGN_PERSON_AND_ORGANIZATION_ASSIGNMENT ( #6381, #7843, ( #10116 ) ) ;
#11957 = VERTEX_POINT ( 'NONE', #8136 ) ;
#11958 = CARTESIAN_POINT ( 'NONE',  ( 4.226910153394439540, 0.3260126676757187369, 0.9376784990094754191 ) ) ;
#11959 = CARTESIAN_POINT ( 'NONE',  ( -1.346194077712558945, 5.062500000000000888, -0.2500000000000002220 ) ) ;
#11960 = AXIS2_PLACEMENT_3D ( 'NONE', #998, #7872, #10427 ) ;
#11961 = CARTESIAN_POINT ( 'NONE',  ( -8.870626307758040952, 2.148733653892300310, -105.5059564705872361 ) ) ;
#11962 = CARTESIAN_POINT ( 'NONE',  ( 0.000000000000000000, 0.4999999999999999445, -0.2500000000000002220 ) ) ;
#11963 = ADVANCED_FACE ( 'NONE', ( #2354 ), #13019, .F. ) ;
#11964 = CARTESIAN_POINT ( 'NONE',  ( -3.249999999999999556, 6.750000000000001776, -3.500000000000000000 ) ) ;
#11965 = CARTESIAN_POINT ( 'NONE',  ( -0.1147110668984741289, 15.00000000000000000, -113.7369025357346572 ) ) ;
#11966 =( BOUNDED_SURFACE ( )  B_SPLINE_SURFACE ( 3, 2, ( 
 ( #4460, #6778, #6703 ),
 ( #5539, #11494, #10325 ),
 ( #5836, #7934, #13902 ),
 ( #4682, #5686, #9397 ),
 ( #10257, #10556, #2211 ),
 ( #10490, #2294, #14988 ),
 ( #15064, #11415, #3370 ),
 ( #8233, #9251, #15222 ),
 ( #1058, #13975, #8082 ),
 ( #11642, #15289, #12806 ),
 ( #833, #1986, #6920 ),
 ( #5766, #9093, #14046 ),
 ( #4386, #13814, #8155 ),
 ( #4612, #14124, #3215 ),
 ( #6999, #10411, #5612 ),
 ( #15145, #12653, #3301 ),
 ( #2068, #9322, #9173 ),
 ( #977, #8009, #12733 ),
 ( #2145, #11561, #12884 ),
 ( #6848, #11714, #1134 ),
 ( #14517, #11857, #3837 ),
 ( #361, #1360, #8380 ) ),
 .UNSPECIFIED., .F., .F., .T. ) 
 B_SPLINE_SURFACE_WITH_KNOTS ( ( 4, 2, 2, 2, 2, 2, 2, 2, 2, 2, 4 ),
 ( 3, 3 ),
 ( -1.623076171293996825E-05, 0.002723859379327837719, 0.005463949520368615448, 0.006148972055628809663, 0.006833994590889003878, 0.007519017126149198094, 0.008204039661409392309, 0.008889062196669586524, 0.009574084731929780739, 0.01025910726718997495, 0.01094412980245017090 ),
 ( 0.000000000000000000, 1.000000000000000000 ),
 .UNSPECIFIED. ) 
 GEOMETRIC_REPRESENTATION_ITEM ( )  RATIONAL_B_SPLINE_SURFACE ( (
 ( 1.000000000000000000, 1.000000000000000000, 1.000000000000000000),
 ( 1.000000000000000000, 0.9999677357533394151, 1.000000000000000000),
 ( 1.000000000000000000, 0.9926659029119584421, 1.000000000000000000),
 ( 1.000000000000000000, 0.9597381185227591427, 1.000000000000000000),
 ( 1.000000000000000000, 0.9342244066884717313, 1.000000000000000000),
 ( 1.000000000000000000, 0.8868441346594281294, 1.000000000000000000),
 ( 1.000000000000000000, 0.8765818554801813045, 1.000000000000000000),
 ( 1.000000000000000000, 0.8543202666023007597, 1.000000000000000000),
 ( 1.000000000000000000, 0.8422878763855655704, 1.000000000000000000),
 ( 1.000000000000000000, 0.8166978392028928502, 1.000000000000000000),
 ( 1.000000000000000000, 0.8031073211395015621, 1.000000000000000000),
 ( 1.000000000000000000, 0.7743109652644618590, 1.000000000000000000),
 ( 1.000000000000000000, 0.7590349308573662857, 1.000000000000000000),
 ( 1.000000000000000000, 0.7272728521985072359, 1.000000000000000000),
 ( 1.000000000000000000, 0.7108161654301946575, 1.000000000000000000),
 ( 1.000000000000000000, 0.6771951971006066051, 1.000000000000000000),
 ( 1.000000000000000000, 0.6600161975495444366, 1.000000000000000000),
 ( 1.000000000000000000, 0.6258845079443411397, 1.000000000000000000),
 ( 1.000000000000000000, 0.6093097763769845798, 1.000000000000000000),
 ( 1.000000000000000000, 0.5793944113054434464, 1.000000000000000000),
 ( 1.000000000000000000, 0.5659315413484863333, 1.000000000000000000),
 ( 1.000000000000000000, 0.5562760308710636981, 1.000000000000000000) ) ) 
 REPRESENTATION_ITEM ( '' )  SURFACE ( )  );
#11967 = EDGE_CURVE ( 'NONE', #5038, #881, #8748, .T. ) ;
#11968 = CARTESIAN_POINT ( 'NONE',  ( 3.421487705324556483, 14.74649280419825637, -0.009165486442489365060 ) ) ;
#11969 = ADVANCED_FACE ( 'NONE', ( #7117 ), #13487, .T. ) ;
#11970 = CARTESIAN_POINT ( 'NONE',  ( 4.190470984303368063, 15.00000000000000000, -127.0204210814509196 ) ) ;
#11971 = CARTESIAN_POINT ( 'NONE',  ( 3.249999999999998668, 2.687500000000000888, -4.846194077712560500 ) ) ;
#11972 = CARTESIAN_POINT ( 'NONE',  ( 3.749999999999999112, 2.312500000000000000, -1.946699141100893149 ) ) ;
#11973 = CARTESIAN_POINT ( 'NONE',  ( -3.750000000000000000, 6.187500000000000000, -1.946699141100892927 ) ) ;
#11974 = DIRECTION ( 'NONE',  ( -0.05964429961207245307, 0.000000000000000000, -0.9982196940171964572 ) ) ;
#11975 = CARTESIAN_POINT ( 'NONE',  ( 3.750000000000000000, 5.312500000000000000, -1.946699141100892705 ) ) ;
#11976 = CARTESIAN_POINT ( 'NONE',  ( 4.015443435590369425, 13.35568666415761285, 3.641580877850956632 ) ) ;
#11977 = DIRECTION ( 'NONE',  ( -0.000000000000000000, 1.000000000000000000, -0.000000000000000000 ) ) ;
#11978 = LINE ( 'NONE', #11898, #719 ) ;
#11979 = CARTESIAN_POINT ( 'NONE',  ( 1.004809442601847236, 5.000000000000000888, -139.4752805618705906 ) ) ;
#11980 = CARTESIAN_POINT ( 'NONE',  ( -3.249999999999999556, 14.18750000000000000, -2.153805922287440833 ) ) ;
#11981 = DIRECTION ( 'NONE',  ( 1.000000000000000000, 0.000000000000000000, 0.000000000000000000 ) ) ;
#11982 = ORIENTED_EDGE ( 'NONE', *, *, #15009, .F. ) ;
#11983 = CARTESIAN_POINT ( 'NONE',  ( -3.749999999999999556, 10.75000000000000000, -3.499999999999999112 ) ) ;
#11984 = VERTEX_POINT ( 'NONE', #6364 ) ;
#11985 = CARTESIAN_POINT ( 'NONE',  ( -5.346294835442622073, -6.653696274010802536E-13, -111.0961406517098027 ) ) ;
#11986 = CARTESIAN_POINT ( 'NONE',  ( -9.742503157198443731, -2.490287375297126626, -40.35209559314896666 ) ) ;
#11987 = CARTESIAN_POINT ( 'NONE',  ( 3.749999999999999112, 9.812500000000000000, -1.946699141100892039 ) ) ;
#11988 = CARTESIAN_POINT ( 'NONE',  ( -4.592425496802573972E-16, 4.000000000000000000, -7.250000000000000000 ) ) ;
#11989 = DIRECTION ( 'NONE',  ( 0.1564344650402314796, 0.000000000000000000, 0.9876883405951375483 ) ) ;
#11990 = ORIENTED_EDGE ( 'NONE', *, *, #3565, .T. ) ;
#11991 = CARTESIAN_POINT ( 'NONE',  ( -1.346194077712559167, 4.937500000000000000, -6.749999999999999112 ) ) ;
#11992 = CC_DESIGN_DATE_AND_TIME_ASSIGNMENT ( #3388, #8099, ( #10180 ) ) ;
#11993 = CARTESIAN_POINT ( 'NONE',  ( -70.09987374419694106, 15.00000000000000000, -191.4540390840448367 ) ) ;
#11994 = CARTESIAN_POINT ( 'NONE',  ( 3.379596559112451271, 8.673617379884035472E-16, -115.6190070853288034 ) ) ;
#11995 = CARTESIAN_POINT ( 'NONE',  ( -3.980102097228897245E-16, 8.500000000000000000, -6.749999999999999112 ) ) ;
#11996 = SECURITY_CLASSIFICATION_LEVEL ( 'unclassified' ) ;
#11997 = CARTESIAN_POINT ( 'NONE',  ( 1.320501113854922082, -4.336808689942017736E-15, -137.8664870916820178 ) ) ;
#11998 = CARTESIAN_POINT ( 'NONE',  ( 6.844193222559625589, 8.673617379884035472E-16, -124.9748991231763000 ) ) ;
#11999 = VERTEX_POINT ( 'NONE', #11076 ) ;
#12000 = LINE ( 'NONE', #11010, #6431 ) ;
#12001 = DIRECTION ( 'NONE',  ( -0.000000000000000000, -1.000000000000000000, -0.000000000000000000 ) ) ;
#12002 = EDGE_LOOP ( 'NONE', ( #9670, #7791, #7945 ) ) ;
#12003 = ORIENTED_EDGE ( 'NONE', *, *, #14045, .T. ) ;
#12004 = CARTESIAN_POINT ( 'NONE',  ( 26.98741591943780094, 4.264362126257767116, -138.2255432259009922 ) ) ;
#12005 = CARTESIAN_POINT ( 'NONE',  ( -3.750000000000000000, 10.81250000000000000, -5.053300858899105741 ) ) ;
#12006 = CARTESIAN_POINT ( 'NONE',  ( 3.249999999999998224, 6.312500000000000000, -2.153805922287439945 ) ) ;
#12007 = CARTESIAN_POINT ( 'NONE',  ( -2.298097038856278029, 8.624999999999998224, -1.201902961143720638 ) ) ;
#12008 = ORIENTED_EDGE ( 'NONE', *, *, #9574, .F. ) ;
#12009 = CARTESIAN_POINT ( 'NONE',  ( -24.07555247732078030, 3.209883240645346926E-32, -197.1572433827812176 ) ) ;
#12010 = CARTESIAN_POINT ( 'NONE',  ( 3.249999999999999112, 5.812500000000000000, -2.153805922287439945 ) ) ;
#12011 = CARTESIAN_POINT ( 'NONE',  ( -6.683304552674626642, 0.000000000000000000, -104.1296019027811894 ) ) ;
#12012 = DIRECTION ( 'NONE',  ( 0.8674617751425299783, 0.000000000000000000, 0.4975038378410468476 ) ) ;
#12013 = EDGE_CURVE ( 'NONE', #1308, #9158, #11220, .T. ) ;
#12014 = EDGE_CURVE ( 'NONE', #8296, #8528, #7593, .T. ) ;
#12015 = CARTESIAN_POINT ( 'NONE',  ( -9.030574454602197321, 2.490287375297123962, -34.97919997656152447 ) ) ;
#12016 = B_SPLINE_CURVE_WITH_KNOTS ( 'NONE', 3,
 ( #5907, #11562, #5687, #2212, #15065, #7935, #9324, #2369, #15146, #2146 ),
 .UNSPECIFIED., .F., .F.,
 ( 4, 2, 2, 2, 4 ),
 ( 3.469446951953614189E-18, 0.009507825141772015265, 0.01901565028354402706, 0.02852347542531603886, 0.03803130056708804718 ),
 .UNSPECIFIED. ) ;
#12017 = PERSON_AND_ORGANIZATION ( #3176, #3020 ) ;
#12018 = B_SPLINE_CURVE_WITH_KNOTS ( 'NONE', 3,
 ( #5505, #7750, #7826, #6666, #14961, #9062, #13784, #3182, #2032, #1241, #4501, #13939, #3488, #12694, #8118, #10589, #2336, #9209, #5949, #8271 ),
 .UNSPECIFIED., .F., .F.,
 ( 4, 2, 2, 2, 2, 2, 2, 2, 2, 4 ),
 ( 0.000000000000000000, 0.001232535436417454789, 0.002465070872834909579, 0.003697606309252364151, 0.004930141745669819157, 0.005546409463878545359, 0.006162677182087270694, 0.007395212618504723098, 0.008627748054922173768, 0.009860283491339624437 ),
 .UNSPECIFIED. ) ;
#12019 = CARTESIAN_POINT ( 'NONE',  ( 0.01496453197139708223, 5.000000000000000000, 5.196130874293197088 ) ) ;
#12020 = AXIS2_PLACEMENT_3D ( 'NONE', #14259, #3658, #8442 ) ;
#12021 = ORIENTED_EDGE ( 'NONE', *, *, #7235, .T. ) ;
#12022 = CARTESIAN_POINT ( 'NONE',  ( -3.249999999999999556, 2.187500000000000444, -2.153805922287440833 ) ) ;
#12023 = DIRECTION ( 'NONE',  ( -0.9997619372588932851, 0.000000000000000000, -0.02181900108494707474 ) ) ;
#12024 = CARTESIAN_POINT ( 'NONE',  ( 3.749999999999999556, 15.25000000000000355, -3.500000000000000444 ) ) ;
#12025 = CARTESIAN_POINT ( 'NONE',  ( -65.01995796243984671, 15.35663992353611995, -206.2218773783315271 ) ) ;
#12026 = CARTESIAN_POINT ( 'NONE',  ( -9.385448347264265578, 9.999999999999998224, -115.3551636530117150 ) ) ;
#12027 = CARTESIAN_POINT ( 'NONE',  ( 3.249999999999999556, 3.250000000000000000, -3.500000000000000000 ) ) ;
#12028 = FACE_OUTER_BOUND ( 'NONE', #12831, .T. ) ;
#12029 = DATE_AND_TIME ( #7315, #1056 ) ;
#12030 = EDGE_CURVE ( 'NONE', #1308, #6835, #6128, .T. ) ;
#12031 = CARTESIAN_POINT ( 'NONE',  ( -8.671560925439079526, 2.743867526398026779, -35.09585054340070798 ) ) ;
#12032 = DIRECTION ( 'NONE',  ( -0.000000000000000000, 1.000000000000000000, -0.000000000000000000 ) ) ;
#12033 = EDGE_LOOP ( 'NONE', ( #9384, #12021, #14424, #14348, #4430, #14219 ) ) ;
#12034 = CARTESIAN_POINT ( 'NONE',  ( 6.896101684162133871, 0.9384448392688442553, 1.465219231324311977 ) ) ;
#12035 = CARTESIAN_POINT ( 'NONE',  ( -2.298097038856278473, 6.125000000000000000, -1.201902961143720416 ) ) ;
#12036 = CARTESIAN_POINT ( 'NONE',  ( -64.97045305008005300, 9.999999999999998224, -167.8253422882257269 ) ) ;
#12037 = CARTESIAN_POINT ( 'NONE',  ( -2.298097038856278473, 14.12500000000000000, -1.201902961143720416 ) ) ;
#12038 = CARTESIAN_POINT ( 'NONE',  ( -3.980102097228897738E-16, 5.000000000000000000, -6.749999999999999112 ) ) ;
#12039 = CARTESIAN_POINT ( 'NONE',  ( -5.418245838931921021, 14.99999999999939071, -110.8346421744157055 ) ) ;
#12040 = DIRECTION ( 'NONE',  ( 0.000000000000000000, 0.000000000000000000, 1.000000000000000000 ) ) ;
#12041 = DIRECTION ( 'NONE',  ( -0.000000000000000000, -1.000000000000000000, -0.000000000000000000 ) ) ;
#12042 = CARTESIAN_POINT ( 'NONE',  ( 1.346194077712558057, 4.562500000000000888, -6.750000000000000000 ) ) ;
#12043 = CARTESIAN_POINT ( 'NONE',  ( -1.553300858899106629, 0.5625000000000001110, 0.2499999999999998335 ) ) ;
#12044 = CARTESIAN_POINT ( 'NONE',  ( -2.651650429449552870, 5.125000000000000000, -0.8483495705504462414 ) ) ;
#12045 = CARTESIAN_POINT ( 'NONE',  ( -3.979893100209070056, 11.11731708281460129, -46.51432482832429116 ) ) ;
#12046 = CARTESIAN_POINT ( 'NONE',  ( -1.553300858899106629, 4.562500000000000000, 0.2500000000000002220 ) ) ;
#12047 = CARTESIAN_POINT ( 'NONE',  ( 3.803251406275964808, 12.89415288025766593, 4.113245758263203378 ) ) ;
#12048 = CARTESIAN_POINT ( 'NONE',  ( 10.67218363251896207, 0.3802680776948408337, -164.3671655685305950 ) ) ;
#12049 = ADVANCED_FACE ( 'NONE', ( #10072 ), #14808, .F. ) ;
#12050 = EDGE_CURVE ( 'NONE', #15191, #9868, #3570, .T. ) ;
#12051 = CARTESIAN_POINT ( 'NONE',  ( -8.589778368047582546, 1.226453351861508612, -105.3195804397573170 ) ) ;
#12052 = EDGE_CURVE ( 'NONE', #587, #5152, #1722, .T. ) ;
#12053 = CARTESIAN_POINT ( 'NONE',  ( -11.06538882243261135, 3.999999999999993783, -149.4796096102432159 ) ) ;
#12054 = DIRECTION ( 'NONE',  ( 0.000000000000000000, 0.000000000000000000, -1.000000000000000000 ) ) ;
#12055 =( BOUNDED_SURFACE ( )  B_SPLINE_SURFACE ( 3, 2, ( 
 ( #238, #8199, #2340 ),
 ( #7103, #4953, #1246 ),
 ( #4805, #7036, #11750 ),
 ( #1172, #5873, #10592 ),
 ( #324, #14483, #12057 ),
 ( #8580, #10905, #5037 ) ),
 .UNSPECIFIED., .F., .F., .F. ) 
 B_SPLINE_SURFACE_WITH_KNOTS ( ( 4, 2, 4 ),
 ( 3, 3 ),
 ( 0.000000000000000000, 0.006940540637791398938, 0.01388108127558279788 ),
 ( 0.000000000000000000, 1.000000000000000000 ),
 .UNSPECIFIED. ) 
 GEOMETRIC_REPRESENTATION_ITEM ( )  RATIONAL_B_SPLINE_SURFACE ( (
 ( 1.000000000000000000, 0.7071067811865469066, 1.000000000000000000),
 ( 1.000000000000000000, 0.7071067811865469066, 1.000000000000000000),
 ( 1.000000000000000000, 0.7071067811865475727, 1.000000000000000000),
 ( 1.000000000000000000, 0.7071067811865475727, 1.000000000000000000),
 ( 1.000000000000000000, 0.7071067811865471286, 1.000000000000000000),
 ( 1.000000000000000000, 0.7071067811865471286, 1.000000000000000000) ) ) 
 REPRESENTATION_ITEM ( '' )  SURFACE ( )  );
#12056 = CARTESIAN_POINT ( 'NONE',  ( -24.07048164010645408, 8.673617379884033500E-16, -181.3206119412710962 ) ) ;
#12057 = CARTESIAN_POINT ( 'NONE',  ( -0.3733149413592447008, 8.673617379884035472E-16, -108.7489923163346361 ) ) ;
#12058 = EDGE_LOOP ( 'NONE', ( #14448, #12008, #13965, #7957 ) ) ;
#12059 = CARTESIAN_POINT ( 'NONE',  ( 3.750000000000000000, 11.31250000000000000, -1.946699141100892705 ) ) ;
#12060 = ORIENTED_EDGE ( 'NONE', *, *, #7409, .T. ) ;
#12061 = CARTESIAN_POINT ( 'NONE',  ( -5.336847315148803617, 9.283940533607051382E-13, -115.5414184961177000 ) ) ;
#12062 = CARTESIAN_POINT ( 'NONE',  ( -0.9087754948914894548, 0.000000000000000000, -45.55632290616385660 ) ) ;
#12063 = CARTESIAN_POINT ( 'NONE',  ( -4.592425496802573972E-16, 7.500000000000000000, -7.249999999999999112 ) ) ;
#12064 = CARTESIAN_POINT ( 'NONE',  ( 1.553300858899109071, 7.437499999999999112, 0.2499999999999989175 ) ) ;
#12065 = CARTESIAN_POINT ( 'NONE',  ( 4.950900406836922230, 0.000000000000000000, -134.4284351762048573 ) ) ;
#12066 = ORIENTED_EDGE ( 'NONE', *, *, #13823, .T. ) ;
#12067 = CARTESIAN_POINT ( 'NONE',  ( -7.978007822721722597, 1.532620112711841509, -115.9805901612375578 ) ) ;
#12068 = CARTESIAN_POINT ( 'NONE',  ( -1.346194077712559167, 2.937500000000000444, -6.749999999999999112 ) ) ;
#12069 = CARTESIAN_POINT ( 'NONE',  ( 2.651650429449553759, 7.875000000000000000, -0.8483495705504471296 ) ) ;
#12070 = CARTESIAN_POINT ( 'NONE',  ( -65.03533772944689417, 15.00000000000000000, -189.5630629144658599 ) ) ;
#12071 = DIRECTION ( 'NONE',  ( 0.000000000000000000, 0.000000000000000000, 1.000000000000000000 ) ) ;
#12072 = CARTESIAN_POINT ( 'NONE',  ( -2.298097038856278473, 6.125000000000000000, -1.201902961143720416 ) ) ;
#12073 = EDGE_CURVE ( 'NONE', #6503, #10677, #8985, .T. ) ;
#12074 = CARTESIAN_POINT ( 'NONE',  ( -5.418138540701907147, 10.00000000000000355, -127.8817495432483469 ) ) ;
#12075 = APPROVAL_DATE_TIME ( #13332, #9706 ) ;
#12076 = CARTESIAN_POINT ( 'NONE',  ( -3.672164062342282875, 4.999999999996045830, -131.0905698958435437 ) ) ;
#12077 = CARTESIAN_POINT ( 'NONE',  ( 10.69730027793196747, 5.000000000000000888, -107.4734661196136472 ) ) ;
#12078 = ORIENTED_EDGE ( 'NONE', *, *, #665, .F. ) ;
#12079 = DIRECTION ( 'NONE',  ( 0.000000000000000000, 0.000000000000000000, 1.000000000000000000 ) ) ;
#12080 = CARTESIAN_POINT ( 'NONE',  ( 30.32986759126112730, 1.750000000000000000, 45.04214087805580391 ) ) ;
#12081 = ORIENTED_EDGE ( 'NONE', *, *, #8437, .T. ) ;
#12082 = ORIENTED_EDGE ( 'NONE', *, *, #8941, .T. ) ;
#12083 = CARTESIAN_POINT ( 'NONE',  ( 25.55817180536042343, 1.743203967168683866, -138.4078944009487486 ) ) ;
#12084 = CARTESIAN_POINT ( 'NONE',  ( 2.651650429449552870, 14.12500000000000000, -6.151650429449553314 ) ) ;
#12085 = CARTESIAN_POINT ( 'NONE',  ( -2.298097038856278029, 12.62500000000000000, -1.201902961143720638 ) ) ;
#12086 = CARTESIAN_POINT ( 'NONE',  ( 2.298097038856279362, 10.37500000000000000, -1.201902961143720860 ) ) ;
#12087 = ORIENTED_EDGE ( 'NONE', *, *, #6609, .T. ) ;
#12088 = FACE_BOUND ( 'NONE', #3967, .T. ) ;
#12089 = CARTESIAN_POINT ( 'NONE',  ( -3.249999999999999556, 6.250000000000000000, -3.499999999999999556 ) ) ;
#12090 = PRODUCT_DEFINITION_FORMATION_WITH_SPECIFIED_SOURCE ( 'ANY', '', #5834, .NOT_KNOWN. ) ;
#12091 = VECTOR ( 'NONE', #3901, 1000.000000000000000 ) ;
#12092 = CARTESIAN_POINT ( 'NONE',  ( -9.103428091817445278, 1.676764629372798465, -104.6332280698933346 ) ) ;
#12093 = DIRECTION ( 'NONE',  ( -0.4975038378410469031, 0.000000000000000000, 0.8674617751425300893 ) ) ;
#12094 = LINE ( 'NONE', #10945, #10888 ) ;
#12095 = DATE_AND_TIME ( #4912, #751 ) ;
#12096 = FACE_BOUND ( 'NONE', #4786, .T. ) ;
#12097 = ORGANIZATION ( 'NAUO-ORG1', 'UNSPECIFIED', 'UNSPECIFIED' ) ;
#12098 = VERTEX_POINT ( 'NONE', #13861 ) ;
#12099 = CARTESIAN_POINT ( 'NONE',  ( -1.346194077712559389, 9.062499999999998224, -0.2500000000000002220 ) ) ;
#12100 = AXIS2_PLACEMENT_3D ( 'NONE', #14398, #3797, #12054 ) ;
#12101 = CARTESIAN_POINT ( 'NONE',  ( 2.298097038856278029, 14.12500000000000000, -5.798097038856279362 ) ) ;
#12102 = CARTESIAN_POINT ( 'NONE',  ( 1.553300858899105963, 14.56250000000000000, -7.250000000000000888 ) ) ;
#12103 = AXIS2_PLACEMENT_3D ( 'NONE', #3794, #1165, #8417 ) ;
#12104 = CIRCLE ( 'NONE', #14604, 3.250000000000003553 ) ;
#12105 = DIRECTION ( 'NONE',  ( 0.000000000000000000, 0.000000000000000000, 1.000000000000000000 ) ) ;
#12106 = CARTESIAN_POINT ( 'NONE',  ( 3.749999999999998668, 14.18750000000000178, -5.053300858899108405 ) ) ;
#12107 = AXIS2_PLACEMENT_3D ( 'NONE', #265, #8447, #3981 ) ;
#12108 = CARTESIAN_POINT ( 'NONE',  ( -63.38919026794945211, 11.42435839034952494, -203.2128261894144998 ) ) ;
#12109 = FACE_OUTER_BOUND ( 'NONE', #12245, .T. ) ;
#12110 = CARTESIAN_POINT ( 'NONE',  ( -2.298097038856279362, 2.875000000000000000, -5.798097038856278473 ) ) ;
#12111 = VECTOR ( 'NONE', #3743, 1000.000000000000000 ) ;
#12112 = CARTESIAN_POINT ( 'NONE',  ( 6.288457687480498493, 8.673617379884035472E-16, -105.0111312234657817 ) ) ;
#12113 = AXIS2_PLACEMENT_3D ( 'NONE', #12997, #5868, #2401 ) ;
#12114 = PERSON_AND_ORGANIZATION ( #3176, #3020 ) ;
#12115 = CARTESIAN_POINT ( 'NONE',  ( -64.29981409993189345, 14.99999998638445931, -182.3649568880052243 ) ) ;
#12116 = DIRECTION ( 'NONE',  ( -0.000000000000000000, -1.000000000000000000, -0.000000000000000000 ) ) ;
#12117 = VERTEX_POINT ( 'NONE', #3113 ) ;
#12118 = CARTESIAN_POINT ( 'NONE',  ( 5.960046513698709525, 0.2792070234823527675, 2.322492007399493463 ) ) ;
#12119 = CARTESIAN_POINT ( 'NONE',  ( -2.298097038856278918, 7.375000000000000888, -5.798097038856277585 ) ) ;
#12120 = CARTESIAN_POINT ( 'NONE',  ( -69.99910782323208025, 9.999999999999996447, -188.8614012312206398 ) ) ;
#12121 = CARTESIAN_POINT ( 'NONE',  ( 0.000000000000000000, 14.00000000000000000, -0.2500000000000002220 ) ) ;
#12122 = CIRCLE ( 'NONE', #5465, 3.500000000000003109 ) ;
#12123 = CARTESIAN_POINT ( 'NONE',  ( -2.298097038856278029, 11.62500000000000000, -1.201902961143720638 ) ) ;
#12124 = EDGE_CURVE ( 'NONE', #9880, #13770, #6594, .T. ) ;
#12125 = DIRECTION ( 'NONE',  ( 1.000000000000000000, 0.000000000000000000, 0.000000000000000000 ) ) ;
#12126 = CARTESIAN_POINT ( 'NONE',  ( 0.2499999999999999445, 5.000000000000000000, -0.2499999999999997780 ) ) ;
#12127 = CARTESIAN_POINT ( 'NONE',  ( 10.30451295169211434, 14.51423292640433438, -106.1859832732645117 ) ) ;
#12128 = EDGE_CURVE ( 'NONE', #4833, #7693, #5579, .T. ) ;
#12129 = CARTESIAN_POINT ( 'NONE',  ( 2.298097038856278473, 5.625000000000000000, -5.798097038856279362 ) ) ;
#12130 = CARTESIAN_POINT ( 'NONE',  ( 3.249999999999998224, 15.18750000000000355, -4.846194077712561388 ) ) ;
#12131 = CARTESIAN_POINT ( 'NONE',  ( -4.592425496802573972E-16, 4.500000000000000888, -7.249999999999999112 ) ) ;
#12132 = CARTESIAN_POINT ( 'NONE',  ( -3.986154284857507779, 10.61173620962768105, -45.11416216203139129 ) ) ;
#12133 = CARTESIAN_POINT ( 'NONE',  ( 2.651650429449554203, 4.375000000000000888, -0.8483495705504471296 ) ) ;
#12134 = CARTESIAN_POINT ( 'NONE',  ( 1.753027082723892072, 13.64326733232996602, 4.258754144511208040 ) ) ;
#12135 = TOROIDAL_SURFACE ( 'NONE', #2271, 2.000000000000011990, 1.000000000000000000 ) ;
#12136 = DIRECTION ( 'NONE',  ( 0.000000000000000000, 1.000000000000000000, 0.000000000000000000 ) ) ;
#12137 = DIRECTION ( 'NONE',  ( 0.000000000000000000, 1.000000000000000000, 0.000000000000000000 ) ) ;
#12138 = DIRECTION ( 'NONE',  ( 0.9989498407774362043, 0.000000000000000000, 0.04581719776170026931 ) ) ;
#12139 = CARTESIAN_POINT ( 'NONE',  ( -13.13002412793078477, 8.673617379884033500E-16, -159.4945871395674146 ) ) ;
#12140 = ORIENTED_EDGE ( 'NONE', *, *, #2241, .F. ) ;
#12141 = CARTESIAN_POINT ( 'NONE',  ( -2.651650429449553314, 13.87500000000000178, -6.151650429449552426 ) ) ;
#12142 = VERTEX_POINT ( 'NONE', #10294 ) ;
#12143 = MANIFOLD_SOLID_BREP ( 'Saliente-Extruir1', #1416 ) ;
#12144 = CYLINDRICAL_SURFACE ( 'NONE', #7753, 0.4999999999999726885 ) ;
#12145 = CARTESIAN_POINT ( 'NONE',  ( -28.26194796053519909, 8.673617379884035472E-16, -205.0068360181388130 ) ) ;
#12146 = CARTESIAN_POINT ( 'NONE',  ( 1.553300858899108849, 10.93750000000000000, 0.2499999999999993616 ) ) ;
#12147 = CARTESIAN_POINT ( 'NONE',  ( -2.651650429449552870, 8.875000000000000000, -6.151650429449552426 ) ) ;
#12148 = CARTESIAN_POINT ( 'NONE',  ( 19.36487844429745309, 1.750000000002257083, 25.27309906096478187 ) ) ;
#12149 = ORIENTED_EDGE ( 'NONE', *, *, #5347, .F. ) ;
#12150 = EDGE_CURVE ( 'NONE', #3728, #13676, #14883, .T. ) ;
#12151 = CARTESIAN_POINT ( 'NONE',  ( -2.298097038856278029, 3.625000000000000888, -1.201902961143720638 ) ) ;
#12152 = ADVANCED_FACE ( 'NONE', ( #575 ), #10149, .F. ) ;
#12153 = CARTESIAN_POINT ( 'NONE',  ( 1.553300858899105963, 11.56249999999999822, -7.250000000000000888 ) ) ;
#12154 = CARTESIAN_POINT ( 'NONE',  ( -59.11471918145669946, 15.00000000000000000, -166.7985135386829825 ) ) ;
#12155 = CARTESIAN_POINT ( 'NONE',  ( -67.58382170693636226, 10.00000000000000000, -204.5178482451963191 ) ) ;
#12156 = CARTESIAN_POINT ( 'NONE',  ( 33.90323114033518692, -4.182108627340793028, -19.28242517164845538 ) ) ;
#12157 = CARTESIAN_POINT ( 'NONE',  ( -3.249999999999999556, 9.187500000000000000, -2.153805922287440833 ) ) ;
#12158 = CARTESIAN_POINT ( 'NONE',  ( -8.249568998231312733, 10.00000000000325606, -121.3053947661622090 ) ) ;
#12159 = APPROVAL_DATE_TIME ( #11006, #6490 ) ;
#12160 = B_SPLINE_CURVE_WITH_KNOTS ( 'NONE', 3,
 ( #12748, #9262, #11654, #3384 ),
 .UNSPECIFIED., .F., .F.,
 ( 4, 4 ),
 ( 0.000000000000000000, 0.0003780032935241441918 ),
 .UNSPECIFIED. ) ;
#12161 = CARTESIAN_POINT ( 'NONE',  ( -2.971798371524276394, 8.673617379884035472E-16, -121.1412956273195078 ) ) ;
#12162 = CARTESIAN_POINT ( 'NONE',  ( 5.201313589241833846, 0.000000000000000000, -106.6450149762817716 ) ) ;
#12163 = ORIENTED_EDGE ( 'NONE', *, *, #839, .F. ) ;
#12164 = DIRECTION ( 'NONE',  ( 0.7859448108640930686, 0.000000000000000000, -0.6182966555592913638 ) ) ;
#12165 = DIRECTION ( 'NONE',  ( -0.6282721832679394325, -4.359514022472389650E-16, 0.7779936141972740860 ) ) ;
#12166 = EDGE_LOOP ( 'NONE', ( #5928, #12624, #10547, #12857 ) ) ;
#12167 = EDGE_LOOP ( 'NONE', ( #2373, #10248 ) ) ;
#12168 = CARTESIAN_POINT ( 'NONE',  ( -2.524281728693007043, 7.379999999999995453, -45.64919840677852392 ) ) ;
#12169 = CARTESIAN_POINT ( 'NONE',  ( 3.749999999999999556, 12.25000000000000000, -3.500000000000000444 ) ) ;
#12170 = VECTOR ( 'NONE', #10333, 1000.000000000000114 ) ;
#12171 = CARTESIAN_POINT ( 'NONE',  ( -3.249999999999999112, 9.687500000000000000, -2.153805922287440833 ) ) ;
#12172 = CARTESIAN_POINT ( 'NONE',  ( 1.346194077712558279, 12.06250000000000000, -6.750000000000000888 ) ) ;
#12173 = EDGE_LOOP ( 'NONE', ( #10476, #11069, #383, #11087 ) ) ;
#12174 = CARTESIAN_POINT ( 'NONE',  ( 1.346194077712560944, 7.937500000000000888, -0.2500000000000010547 ) ) ;
#12175 = ADVANCED_FACE ( 'NONE', ( #11233 ), #7894, .F. ) ;
#12176 = CARTESIAN_POINT ( 'NONE',  ( 12.51467606204868055, 14.43297906408152542, -125.8675091911941593 ) ) ;
#12177 = CARTESIAN_POINT ( 'NONE',  ( -44.98973890129524733, 10.00000000000000000, -160.2063470242129313 ) ) ;
#12178 = CARTESIAN_POINT ( 'NONE',  ( -44.53431849203957427, 15.00000000000000178, -153.9513641047110468 ) ) ;
#12179 = VECTOR ( 'NONE', #13345, 1000.000000000000000 ) ;
#12180 = DATE_AND_TIME ( #1363, #14834 ) ;
#12181 = CARTESIAN_POINT ( 'NONE',  ( 2.159942170319879562, 5.000000000000000888, -121.5147849362692369 ) ) ;
#12182 = ORIENTED_EDGE ( 'NONE', *, *, #14749, .T. ) ;
#12183 = CARTESIAN_POINT ( 'NONE',  ( -3.249999999999999556, 1.250000000000000000, -3.499999999999999556 ) ) ;
#12184 = CARTESIAN_POINT ( 'NONE',  ( -2.651650429449552870, 13.12500000000000000, -0.8483495705504462414 ) ) ;
#12185 = ORIENTED_EDGE ( 'NONE', *, *, #6101, .T. ) ;
#12186 = CARTESIAN_POINT ( 'NONE',  ( -6.256102584674404277, 1.750000000000027756, 8.120257307136867553 ) ) ;
#12187 = AXIS2_PLACEMENT_3D ( 'NONE', #5536, #10255, #3138 ) ;
#12188 = CIRCLE ( 'NONE', #9959, 0.4999999999999865663 ) ;
#12189 = CARTESIAN_POINT ( 'NONE',  ( 2.651650429449553759, 1.875000000000000000, -0.8483495705504471296 ) ) ;
#12190 = CARTESIAN_POINT ( 'NONE',  ( -64.63350576884886323, 14.96734299377280841, -207.9870121967235264 ) ) ;
#12191 = CARTESIAN_POINT ( 'NONE',  ( -13.94843458185677676, 7.499999999999991118, -95.45326364538628638 ) ) ;
#12192 = CARTESIAN_POINT ( 'NONE',  ( -3.750000000000000000, 1.250000000000000000, -3.499999999999999112 ) ) ;
#12193 = APPROVAL_STATUS ( 'not_yet_approved' ) ;
#12194 = CARTESIAN_POINT ( 'NONE',  ( -25.82983890416511841, 5.000000000000000000, -142.4527639562402328 ) ) ;
#12195 = MANIFOLD_SOLID_BREP ( 'Cortar-Extruir4', #1662 ) ;
#12196 = CIRCLE ( 'NONE', #10975, 3.000000000000011990 ) ;
#12197 = CARTESIAN_POINT ( 'NONE',  ( 9.044950117654433797, 4.000000000000000000, -141.4826476090360643 ) ) ;
#12198 = EDGE_LOOP ( 'NONE', ( #15211, #615, #963, #14847 ) ) ;
#12199 = CARTESIAN_POINT ( 'NONE',  ( 7.867579639100686251, 1.761783548405282618, 4.595106300331015525 ) ) ;
#12200 = CARTESIAN_POINT ( 'NONE',  ( 2.298097038856279362, 7.875000000000000000, -1.201902961143720860 ) ) ;
#12201 = CARTESIAN_POINT ( 'NONE',  ( -8.886921395968292003, 2.324218168650201921, -105.5168766101546822 ) ) ;
#12202 = CARTESIAN_POINT ( 'NONE',  ( -3.249999999999999556, 13.25000000000000000, -3.499999999999999556 ) ) ;
#12203 = CARTESIAN_POINT ( 'NONE',  ( 3.249999999999998224, 11.31250000000000000, -2.153805922287439945 ) ) ;
#12204 = CARTESIAN_POINT ( 'NONE',  ( 7.148068729939693000, 2.490287375297123962, -34.56909192082981974 ) ) ;
#12205 = LINE ( 'NONE', #1911, #7990 ) ;
#12206 = CARTESIAN_POINT ( 'NONE',  ( 28.48375933933716198, 7.321094445766561876, -22.19653139158566901 ) ) ;
#12207 = CARTESIAN_POINT ( 'NONE',  ( -3.249999999999999556, 6.187500000000000888, -2.153805922287440833 ) ) ;
#12208 = VECTOR ( 'NONE', #10493, 1000.000000000000000 ) ;
#12209 = CARTESIAN_POINT ( 'NONE',  ( -3.750000000000000000, 4.812500000000000000, -5.053300858899105741 ) ) ;
#12210 = CARTESIAN_POINT ( 'NONE',  ( 2.651650429449552870, 8.625000000000000000, -6.151650429449554203 ) ) ;
#12211 = CARTESIAN_POINT ( 'NONE',  ( -3.332125411039841723, 10.29294005234724629, -44.11502048402191889 ) ) ;
#12212 = CARTESIAN_POINT ( 'NONE',  ( -3.750000000000000000, 4.687500000000000888, -1.946699141100893149 ) ) ;
#12213 = CARTESIAN_POINT ( 'NONE',  ( 3.243186333997263748, 10.51133653125105027, 5.185517934909010584 ) ) ;
#12214 = CARTESIAN_POINT ( 'NONE',  ( 12.03942984618162626, 1.499941477806701062, -165.3693158247522206 ) ) ;
#12215 = EDGE_CURVE ( 'NONE', #7043, #4897, #5287, .T. ) ;
#12216 = EDGE_CURVE ( 'NONE', #6769, #6645, #14198, .T. ) ;
#12217 = VECTOR ( 'NONE', #10274, 999.9999999999998863 ) ;
#12218 = CARTESIAN_POINT ( 'NONE',  ( 4.030605408878820128, 0.000000000000000000, 7.295648618995377532 ) ) ;
#12219 = CARTESIAN_POINT ( 'NONE',  ( -11.03583607032509306, 8.673617379884034486E-16, -150.6360199482514304 ) ) ;
#12220 = CARTESIAN_POINT ( 'NONE',  ( 3.249999999999999556, 14.75000000000000178, -3.500000000000000000 ) ) ;
#12221 = CARTESIAN_POINT ( 'NONE',  ( -25.66265810730576291, 8.673617379884035472E-16, -195.5605329225483331 ) ) ;
#12222 = ORIENTED_EDGE ( 'NONE', *, *, #14167, .F. ) ;
#12223 = CARTESIAN_POINT ( 'NONE',  ( -2.298097038856278029, 0.6250000000000002220, -1.201902961143720638 ) ) ;
#12224 = ORIENTED_EDGE ( 'NONE', *, *, #7140, .T. ) ;
#12225 = DIRECTION ( 'NONE',  ( -0.08794243244722427244, 0.000000000000000000, -0.9961255586397056438 ) ) ;
#12226 = CARTESIAN_POINT ( 'NONE',  ( -22.78288617575325148, 3.999999999999503064, -204.9228294213145887 ) ) ;
#12227 = CARTESIAN_POINT ( 'NONE',  ( -2.651650429449552870, 10.12500000000000000, -0.8483495705504462414 ) ) ;
#12228 = CARTESIAN_POINT ( 'NONE',  ( 3.749999999999999112, 8.312500000000003553, -1.946699141100893149 ) ) ;
#12229 = CYLINDRICAL_SURFACE ( 'NONE', #13192, 6.999999999999999112 ) ;
#12230 = ORIENTED_EDGE ( 'NONE', *, *, #10183, .F. ) ;
#12231 = CARTESIAN_POINT ( 'NONE',  ( -9.513824166154098094, 3.588159064070329585, -116.4115394435343802 ) ) ;
#12232 = CARTESIAN_POINT ( 'NONE',  ( -3.980102097228897738E-16, 3.000000000000000444, -6.749999999999999112 ) ) ;
#12233 = CARTESIAN_POINT ( 'NONE',  ( 3.749999999999998668, 9.687500000000000000, -5.053300858899107517 ) ) ;
#12234 = CARTESIAN_POINT ( 'NONE',  ( -55.59493099310168418, 15.00000000000000000, -159.7812792143957950 ) ) ;
#12235 = DIRECTION ( 'NONE',  ( 0.000000000000000000, 0.8090169943749465631, -0.5877852522924742473 ) ) ;
#12236 = MECHANICAL_CONTEXT ( 'NONE', #8779, 'mechanical' ) ;
#12237 = CARTESIAN_POINT ( 'NONE',  ( 0.000000000000000000, 8.000000000000000000, -0.2500000000000002220 ) ) ;
#12238 = CARTESIAN_POINT ( 'NONE',  ( -7.397953522037811425, 10.00000000000000000, -106.9836120658180221 ) ) ;
#12239 = EDGE_CURVE ( 'NONE', #9908, #9024, #13638, .T. ) ;
#12240 = CARTESIAN_POINT ( 'NONE',  ( 3.725927156403949780, -8.673617379884035472E-16, -133.0470886511550930 ) ) ;
#12241 = CARTESIAN_POINT ( 'NONE',  ( -97.87133648009834985, 5.000000000000000000, -184.9876713694881971 ) ) ;
#12242 = ORIENTED_EDGE ( 'NONE', *, *, #2538, .T. ) ;
#12243 = FACE_OUTER_BOUND ( 'NONE', #6824, .T. ) ;
#12244 = CARTESIAN_POINT ( 'NONE',  ( 7.781170200712294260, 5.000000000000000888, -20.49502329017444424 ) ) ;
#12245 = EDGE_LOOP ( 'NONE', ( #7017, #5237, #7037, #7207 ) ) ;
#12246 = CARTESIAN_POINT ( 'NONE',  ( -1.376260179405574435, 10.00000000000000178, -106.6458321843530541 ) ) ;
#12247 = CARTESIAN_POINT ( 'NONE',  ( -2.256557393256121369, 7.321094445766562764, -25.56006732368493317 ) ) ;
#12248 = CARTESIAN_POINT ( 'NONE',  ( -2.651650429449552870, 11.87500000000000000, -6.151650429449552426 ) ) ;
#12249 = CARTESIAN_POINT ( 'NONE',  ( -3.249999999999999556, 12.75000000000000178, -3.500000000000000000 ) ) ;
#12250 = CARTESIAN_POINT ( 'NONE',  ( -3.249999999999999112, 13.81250000000000178, -4.846194077712558723 ) ) ;
#12251 = ORIENTED_EDGE ( 'NONE', *, *, #2891, .T. ) ;
#12252 = CARTESIAN_POINT ( 'NONE',  ( -25.11906781955738310, 0.000000000000000000, -198.9681998140721078 ) ) ;
#12253 = CARTESIAN_POINT ( 'NONE',  ( -2.298097038856278918, 6.375000000000000888, -5.798097038856277585 ) ) ;
#12254 = DIRECTION ( 'NONE',  ( 1.000000000000000000, 0.000000000000000000, 0.000000000000000000 ) ) ;
#12255 = DIRECTION ( 'NONE',  ( 0.000000000000000000, -0.000000000000000000, 1.000000000000000000 ) ) ;
#12256 = CARTESIAN_POINT ( 'NONE',  ( -4.234402844927157794, 15.00000000000000000, -117.4888040839639558 ) ) ;
#12257 = CALENDAR_DATE ( 2026, 8, 10 ) ;
#12258 = EDGE_CURVE ( 'NONE', #2743, #2896, #12386, .T. ) ;
#12259 = CARTESIAN_POINT ( 'NONE',  ( -24.65477654877672720, 3.556530958261907127, -208.7318555042168668 ) ) ;
#12260 = EDGE_CURVE ( 'NONE', #5136, #12677, #5357, .T. ) ;
#12261 = EDGE_CURVE ( 'NONE', #11845, #6503, #8910, .T. ) ;
#12262 = EDGE_LOOP ( 'NONE', ( #14070, #8556, #11441, #14941 ) ) ;
#12263 = CARTESIAN_POINT ( 'NONE',  ( 1.346194077712561166, 13.43750000000000178, -0.2500000000000011102 ) ) ;
#12264 = CARTESIAN_POINT ( 'NONE',  ( 2.651650429449553759, 13.87500000000000000, -0.8483495705504471296 ) ) ;
#12265 = EDGE_LOOP ( 'NONE', ( #8524, #13397, #4840, #9347 ) ) ;
#12266 = CARTESIAN_POINT ( 'NONE',  ( -9.030574454602195544, -2.490287375297124850, -34.97919997656152447 ) ) ;
#12267 = APPROVAL ( #14127, 'UNSPECIFIED' ) ;
#12268 = CARTESIAN_POINT ( 'NONE',  ( 3.749999999999999112, 0.8125000000000001110, -1.946699141100892039 ) ) ;
#12269 = CARTESIAN_POINT ( 'NONE',  ( 7.434948248173551377, 5.000000000000000888, -26.28946758364566705 ) ) ;
#12270 = CARTESIAN_POINT ( 'NONE',  ( 0.2073968263107874854, 3.339926503753445797, 2.349187686996549562 ) ) ;
#12271 = AXIS2_PLACEMENT_3D ( 'NONE', #12246, #6369, #14966 ) ;
#12272 = CARTESIAN_POINT ( 'NONE',  ( -2.651650429449552870, 0.1250000000000000278, -0.8483495705504462414 ) ) ;
#12273 = PERSON_AND_ORGANIZATION ( #3176, #3020 ) ;
#12274 = CARTESIAN_POINT ( 'NONE',  ( -67.58763313223541047, 10.54847312031630580, -204.4506847024756837 ) ) ;
#12275 = PLANE ( 'NONE',  #7672 ) ;
#12276 = ORIENTED_EDGE ( 'NONE', *, *, #1963, .F. ) ;
#12277 = CARTESIAN_POINT ( 'NONE',  ( 1.346194077712558279, 7.562500000000000000, -6.750000000000000000 ) ) ;
#12278 = CARTESIAN_POINT ( 'NONE',  ( 0.000000000000000000, 1.000000000000000000, -3.500000000000000000 ) ) ;
#12279 = CARTESIAN_POINT ( 'NONE',  ( -1.346194077712559389, 14.06249999999999822, -0.2500000000000002220 ) ) ;
#12280 = CARTESIAN_POINT ( 'NONE',  ( 1.346194077712561166, 12.43750000000000000, -0.2500000000000011102 ) ) ;
#12281 = CARTESIAN_POINT ( 'NONE',  ( 5.570677809474934072, 7.976916236371252995E-16, -141.9062416701571863 ) ) ;
#12282 = CARTESIAN_POINT ( 'NONE',  ( -12.27209645382209580, 4.336808689942017736E-16, -127.2227734861304782 ) ) ;
#12283 = CARTESIAN_POINT ( 'NONE',  ( 3.249999999999998668, 3.687500000000000444, -4.846194077712560500 ) ) ;
#12284 = CARTESIAN_POINT ( 'NONE',  ( 1.553300858899109071, 3.437500000000000444, 0.2499999999999989175 ) ) ;
#12285 = CARTESIAN_POINT ( 'NONE',  ( 1.553300858899105963, 9.562500000000000000, -7.250000000000000000 ) ) ;
#12286 = CARTESIAN_POINT ( 'NONE',  ( -8.256868333794509240, 1.840915534571258450, -115.8592241392985045 ) ) ;
#12287 = CARTESIAN_POINT ( 'NONE',  ( -3.711477763885599135, 9.806857087768287684, -47.72551489695253224 ) ) ;
#12288 = CARTESIAN_POINT ( 'NONE',  ( -1.553300858899106629, 11.56250000000000178, 0.2500000000000002220 ) ) ;
#12289 = CARTESIAN_POINT ( 'NONE',  ( 4.391429576616724617, 15.00018009634376170, -1.240770632640158411 ) ) ;
#12290 = CARTESIAN_POINT ( 'NONE',  ( 11.61838904370529235, 1.298284280916856659, -165.5431421116371382 ) ) ;
#12291 = DIRECTION ( 'NONE',  ( 0.08794243244722413366, 0.000000000000000000, 0.9961255586397056438 ) ) ;
#12292 = CARTESIAN_POINT ( 'NONE',  ( -25.90868989253521448, 3.999999999998550937, -171.8621034424046172 ) ) ;
#12293 = CARTESIAN_POINT ( 'NONE',  ( -1.302272502657875197, 1.750000000000000000, -1.200882754745186798 ) ) ;
#12294 = LINE ( 'NONE', #9753, #13841 ) ;
#12295 = CARTESIAN_POINT ( 'NONE',  ( -4.592425496802573972E-16, 12.00000000000000178, -7.250000000000000000 ) ) ;
#12296 = ORIENTED_EDGE ( 'NONE', *, *, #14787, .F. ) ;
#12297 = DIRECTION ( 'NONE',  ( 0.9972730031336837220, 0.000000000000000000, -0.07380079417407094111 ) ) ;
#12298 = CARTESIAN_POINT ( 'NONE',  ( -3.749999999999999556, 8.312500000000000000, -5.053300858899104853 ) ) ;
#12299 = CARTESIAN_POINT ( 'NONE',  ( 0.000000000000000000, 7.499999999999999112, 0.2499999999999998057 ) ) ;
#12300 = CARTESIAN_POINT ( 'NONE',  ( -3.482821260068073688, 10.52211603452352939, -46.42594311958101372 ) ) ;
#12301 = CARTESIAN_POINT ( 'NONE',  ( -1.346194077712558945, 6.562500000000000888, -0.2500000000000002220 ) ) ;
#12302 = CARTESIAN_POINT ( 'NONE',  ( 3.749999999999999112, 14.81250000000000000, -1.946699141100892039 ) ) ;
#12303 = CARTESIAN_POINT ( 'NONE',  ( -63.72167557989842379, 15.00000000000000000, -200.9893488412410250 ) ) ;
#12304 = CARTESIAN_POINT ( 'NONE',  ( -8.090126491280004828, -1.779437631024875872E-15, -136.8653377734624996 ) ) ;
#12305 = APPROVAL_STATUS ( 'not_yet_approved' ) ;
#12306 = CARTESIAN_POINT ( 'NONE',  ( 3.249999999999999112, 10.81250000000000178, -2.153805922287439945 ) ) ;
#12307 = CARTESIAN_POINT ( 'NONE',  ( -0.5793326530874192137, 2.529993217055222843, -43.47630266472464911 ) ) ;
#12308 = DIRECTION ( 'NONE',  ( 0.000000000000000000, 0.000000000000000000, 1.000000000000000000 ) ) ;
#12309 = CARTESIAN_POINT ( 'NONE',  ( 6.913513084311236234, 8.673617379884035472E-16, -104.1914153500056841 ) ) ;
#12310 = DIRECTION ( 'NONE',  ( 0.000000000000000000, 0.000000000000000000, 1.000000000000000000 ) ) ;
#12311 = CARTESIAN_POINT ( 'NONE',  ( -25.66911763371813038, 5.000000000000000888, -138.9799121221676046 ) ) ;
#12312 = ORIENTED_EDGE ( 'NONE', *, *, #12337, .T. ) ;
#12313 = CARTESIAN_POINT ( 'NONE',  ( 10.96001082017541250, 5.773884165125716450, -44.27064591564993634 ) ) ;
#12314 = CARTESIAN_POINT ( 'NONE',  ( 24.37641090407976208, 0.8825362985825043749, -138.5554241525009047 ) ) ;
#12315 = CARTESIAN_POINT ( 'NONE',  ( -3.749999999999999556, 10.75000000000000178, -3.499999999999999112 ) ) ;
#12316 = CARTESIAN_POINT ( 'NONE',  ( -3.980102097228897738E-16, 10.00000000000000000, -6.749999999999999112 ) ) ;
#12317 = CARTESIAN_POINT ( 'NONE',  ( 0.000000000000000000, 2.000000000000000000, -0.2500000000000002220 ) ) ;
#12318 = ORIENTED_EDGE ( 'NONE', *, *, #2158, .T. ) ;
#12319 = EDGE_CURVE ( 'NONE', #12098, #13498, #12018, .T. ) ;
#12320 = CARTESIAN_POINT ( 'NONE',  ( -1.346194077712559389, 9.062499999999998224, -0.2500000000000002220 ) ) ;
#12321 = ADVANCED_FACE ( 'NONE', ( #15185 ), #6884, .F. ) ;
#12322 = CARTESIAN_POINT ( 'NONE',  ( 9.976640234167886589, 12.67883206573310062, -45.13187004413220649 ) ) ;
#12323 = CARTESIAN_POINT ( 'NONE',  ( -4.710171483686392158, 15.00000000000000178, -103.4584432832766794 ) ) ;
#12324 = CARTESIAN_POINT ( 'NONE',  ( -0.3766621274091715987, -0.2500000000000000000, -6.863050255469941519 ) ) ;
#12325 = CARTESIAN_POINT ( 'NONE',  ( -9.721966606232506081, 10.36359568089365979, -116.3614657645881323 ) ) ;
#12326 = APPROVAL_STATUS ( 'not_yet_approved' ) ;
#12327 = CARTESIAN_POINT ( 'NONE',  ( 4.544676675852343806, 6.000000000000000000, -126.1782412829290934 ) ) ;
#12328 = CC_DESIGN_PERSON_AND_ORGANIZATION_ASSIGNMENT ( #13597, #6469, ( #5003 ) ) ;
#12329 = ORIENTED_EDGE ( 'NONE', *, *, #8163, .F. ) ;
#12330 = CARTESIAN_POINT ( 'NONE',  ( -3.980102097228897738E-16, 14.00000000000000000, -6.749999999999999112 ) ) ;
#12331 = CARTESIAN_POINT ( 'NONE',  ( -3.750000000000000000, -0.1874999999999998890, -5.053300858899105741 ) ) ;
#12332 = VERTEX_POINT ( 'NONE', #3408 ) ;
#12333 = PRODUCT_DEFINITION_FORMATION_WITH_SPECIFIED_SOURCE ( 'ANY', '', #12881, .NOT_KNOWN. ) ;
#12334 = AXIS2_PLACEMENT_3D ( 'NONE', #9669, #10675, #11683 ) ;
#12335 = ADVANCED_FACE ( 'NONE', ( #11680 ), #9671, .T. ) ;
#12336 = CARTESIAN_POINT ( 'NONE',  ( 0.000000000000000000, 3.061616997868383018E-17, 0.2500000000000002220 ) ) ;
#12337 = EDGE_CURVE ( 'NONE', #6374, #10593, #89, .T. ) ;
#12338 = LINE ( 'NONE', #2998, #1217 ) ;
#12339 = CARTESIAN_POINT ( 'NONE',  ( 0.1512067241414354890, 2.824897904590649933, 1.712721360606747956 ) ) ;
#12340 = CARTESIAN_POINT ( 'NONE',  ( 11.14414536921188592, 3.613765879947322013, -106.7459647845625597 ) ) ;
#12341 = PERSON_AND_ORGANIZATION ( #3176, #3020 ) ;
#12342 = CC_DESIGN_APPROVAL ( #13108, ( #7654 ) ) ;
#12343 = CARTESIAN_POINT ( 'NONE',  ( -16.51872302133460124, 0.000000000000000000, -108.9020125831789727 ) ) ;
#12344 = DIRECTION ( 'NONE',  ( 0.7220210382022057560, 0.000000000000000000, -0.6918711009959940261 ) ) ;
#12345 = B_SPLINE_CURVE_WITH_KNOTS ( 'NONE', 3,
 ( #5573, #8902, #5350, #13854 ),
 .UNSPECIFIED., .F., .F.,
 ( 4, 4 ),
 ( 0.06025750390222917030, 0.06449836217413487671 ),
 .UNSPECIFIED. ) ;
#12346 = ORIENTED_EDGE ( 'NONE', *, *, #13384, .F. ) ;
#12347 = CARTESIAN_POINT ( 'NONE',  ( -3.249999999999999556, 10.25000000000000000, -3.499999999999999556 ) ) ;
#12348 = CARTESIAN_POINT ( 'NONE',  ( 1.320501113854927633, 6.000000000000000000, -137.8664870916819893 ) ) ;
#12349 = CARTESIAN_POINT ( 'NONE',  ( 3.249999999999999556, 2.249999999999999556, -3.500000000000000000 ) ) ;
#12350 = CARTESIAN_POINT ( 'NONE',  ( -3.249999999999999112, 12.68750000000000000, -2.153805922287440833 ) ) ;
#12351 = CARTESIAN_POINT ( 'NONE',  ( 2.530298019944476451, 2.500000000000000888, 0.2330448234422073106 ) ) ;
#12352 = CIRCLE ( 'NONE', #14608, 0.4999999999999726885 ) ;
#12353 = CARTESIAN_POINT ( 'NONE',  ( 11.04869015131055399, 13.64261357365585070, -106.3489331929075519 ) ) ;
#12354 = CARTESIAN_POINT ( 'NONE',  ( -1.346194077712559389, 3.062500000000000000, -0.2500000000000002220 ) ) ;
#12355 = CARTESIAN_POINT ( 'NONE',  ( 1.553300858899105963, 5.062500000000000000, -7.249999999999999112 ) ) ;
#12356 = VECTOR ( 'NONE', #5281, 1000.000000000000114 ) ;
#12357 = EDGE_CURVE ( 'NONE', #13477, #12980, #8130, .T. ) ;
#12358 = AXIS2_PLACEMENT_3D ( 'NONE', #14288, #9645, #2384 ) ;
#12359 = CARTESIAN_POINT ( 'NONE',  ( -3.750000000000000000, 11.25000000000000000, -3.499999999999999112 ) ) ;
#12360 = FACE_OUTER_BOUND ( 'NONE', #7977, .T. ) ;
#12361 = CARTESIAN_POINT ( 'NONE',  ( 33.75578156417348907, -2.051692149508337651E-14, 39.47650855366865841 ) ) ;
#12362 = CARTESIAN_POINT ( 'NONE',  ( -3.750000000000000000, 9.812500000000000000, -5.053300858899105741 ) ) ;
#12363 = CARTESIAN_POINT ( 'NONE',  ( 9.044950117654433797, 0.000000000000000000, -141.4826476090360643 ) ) ;
#12364 = CARTESIAN_POINT ( 'NONE',  ( 0.000000000000000000, 0.000000000000000000, 0.000000000000000000 ) ) ;
#12365 = CARTESIAN_POINT ( 'NONE',  ( 0.000000000000000000, 4.000000000000000000, -3.500000000000000000 ) ) ;
#12366 = VECTOR ( 'NONE', #1929, 1000.000000000000114 ) ;
#12367 = CARTESIAN_POINT ( 'NONE',  ( -9.094017300323571362, 8.673617379884035472E-16, -154.5612483065650054 ) ) ;
#12368 = CARTESIAN_POINT ( 'NONE',  ( 5.824043469730588285, 0.03107126107963375031, -140.0877662325354436 ) ) ;
#12369 = DESIGN_CONTEXT ( 'detailed design', #5610, 'design' ) ;
#12370 = CARTESIAN_POINT ( 'NONE',  ( -25.11906781955738310, 0.000000000000000000, -198.9681998140721078 ) ) ;
#12371 = CARTESIAN_POINT ( 'NONE',  ( -1.553300858899107073, 13.93750000000000000, -7.249999999999999112 ) ) ;
#12372 = ORIENTED_EDGE ( 'NONE', *, *, #4765, .F. ) ;
#12373 = PLANE ( 'NONE',  #14395 ) ;
#12374 = CARTESIAN_POINT ( 'NONE',  ( 10.25880996898554542, 1.911678198002125573, -106.0927282050041640 ) ) ;
#12375 = CARTESIAN_POINT ( 'NONE',  ( -2.651650429449552870, 9.624999999999998224, -0.8483495705504467965 ) ) ;
#12376 = CARTESIAN_POINT ( 'NONE',  ( 26.58801926426210116, 6.000000000000000000, -139.0072983920785532 ) ) ;
#12377 = CARTESIAN_POINT ( 'NONE',  ( 1.346194077712558279, 8.062500000000001776, -6.750000000000000888 ) ) ;
#12378 = DIRECTION ( 'NONE',  ( 0.000000000000000000, 0.000000000000000000, -1.000000000000000000 ) ) ;
#12379 = CARTESIAN_POINT ( 'NONE',  ( 1.553300858899108849, 13.93750000000000000, 0.2499999999999993616 ) ) ;
#12380 = SHAPE_REPRESENTATION ( 'PruningShears-Part2_Predeterminado', ( #9419 ), #11867 ) ;
#12381 = CARTESIAN_POINT ( 'NONE',  ( -68.36774365628944850, 15.00000000000000000, -202.8408623584168140 ) ) ;
#12382 = CARTESIAN_POINT ( 'NONE',  ( 0.3766621274091721538, 0.3292059843107342232, -7.146945437571387671 ) ) ;
#12383 = PERSON_AND_ORGANIZATION_ROLE ( 'creator' ) ;
#12384 = CARTESIAN_POINT ( 'NONE',  ( -1.346194077712559389, 10.06250000000000000, -0.2500000000000002220 ) ) ;
#12385 = CARTESIAN_POINT ( 'NONE',  ( -9.742503157198449060, 2.490287375297123962, -40.35209559314896666 ) ) ;
#12386 = LINE ( 'NONE', #13714, #10723 ) ;
#12387 = CARTESIAN_POINT ( 'NONE',  ( 7.608837862079233183, 8.673617379884035472E-16, -103.4801572790971846 ) ) ;
#12388 = DIRECTION ( 'NONE',  ( 0.000000000000000000, 1.000000000000000000, 0.000000000000000000 ) ) ;
#12389 = CARTESIAN_POINT ( 'NONE',  ( -0.2500000000000000555, 5.000000000000000000, 1.500000000000000222 ) ) ;
#12390 = APPROVAL_PERSON_ORGANIZATION ( #15161, #8378, #4558 ) ;
#12391 = ORIENTED_EDGE ( 'NONE', *, *, #8870, .T. ) ;
#12392 = FACE_OUTER_BOUND ( 'NONE', #6798, .T. ) ;
#12393 = CARTESIAN_POINT ( 'NONE',  ( 4.492499072540838689, 5.000000000000000000, -2.611025101989581820 ) ) ;
#12394 = CARTESIAN_POINT ( 'NONE',  ( 0.000000000000000000, 1.000000000000000000, 0.2500000000000002220 ) ) ;
#12395 = CARTESIAN_POINT ( 'NONE',  ( 2.298097038856279362, 12.37500000000000178, -1.201902961143720860 ) ) ;
#12396 = CARTESIAN_POINT ( 'NONE',  ( 1.346194077712558279, 13.06249999999999822, -6.750000000000000888 ) ) ;
#12397 = ORIENTED_EDGE ( 'NONE', *, *, #9125, .F. ) ;
#12398 = CARTESIAN_POINT ( 'NONE',  ( -1.346194077712559389, 11.06250000000000000, -0.2500000000000002220 ) ) ;
#12399 = LINE ( 'NONE', #11167, #7153 ) ;
#12400 = APPROVAL_PERSON_ORGANIZATION ( #12114, #8931, #4012 ) ;
#12401 = CARTESIAN_POINT ( 'NONE',  ( 13.68910679601487246, 13.48624612131195555, -126.1906338203120157 ) ) ;
#12402 = CARTESIAN_POINT ( 'NONE',  ( 5.942951940282705792, 3.392001843152369300, 5.005362280283235599 ) ) ;
#12403 = LINE ( 'NONE', #820, #10639 ) ;
#12404 = PERSON_AND_ORGANIZATION ( #3176, #3020 ) ;
#12405 = CARTESIAN_POINT ( 'NONE',  ( 8.821381957564753407, 15.00000000000000000, -110.6350233297983436 ) ) ;
#12406 = AXIS2_PLACEMENT_3D ( 'NONE', #5566, #3325, #12678 ) ;
#12407 = EDGE_LOOP ( 'NONE', ( #7547, #15036, #3595, #195 ) ) ;
#12408 = EDGE_CURVE ( 'NONE', #1063, #7480, #2846, .T. ) ;
#12409 = CARTESIAN_POINT ( 'NONE',  ( -1.346194077712559389, 6.062500000000000000, -0.2500000000000002220 ) ) ;
#12410 = CARTESIAN_POINT ( 'NONE',  ( -0.2993152428870710091, 4.000000000000000000, -140.3884260891180418 ) ) ;
#12411 = CARTESIAN_POINT ( 'NONE',  ( 3.749999999999998668, 14.68750000000000000, -5.053300858899107517 ) ) ;
#12412 = ORIENTED_EDGE ( 'NONE', *, *, #1019, .T. ) ;
#12413 = CARTESIAN_POINT ( 'NONE',  ( -6.865783330443320231, 1.750000000000649258, 20.65929969372286479 ) ) ;
#12414 = CARTESIAN_POINT ( 'NONE',  ( -2.651650429449552870, 3.125000000000000000, -0.8483495705504462414 ) ) ;
#12415 = TOROIDAL_SURFACE ( 'NONE', #3048, 2.250000000000003553, 1.000000000000000000 ) ;
#12416 = DIRECTION ( 'NONE',  ( 0.000000000000000000, 0.000000000000000000, -1.000000000000000000 ) ) ;
#12417 = CARTESIAN_POINT ( 'NONE',  ( 0.1555198618414440070, 0.03945862746746779670, 1.761576351096415749 ) ) ;
#12418 = CARTESIAN_POINT ( 'NONE',  ( -6.288157641191917335, 6.000000000000000000, -124.9981450708252595 ) ) ;
#12419 = PERSON_AND_ORGANIZATION ( #3176, #3020 ) ;
#12420 = CARTESIAN_POINT ( 'NONE',  ( 9.801515392239481983, 5.000000000000000000, -108.6954945137553494 ) ) ;
#12421 = DIRECTION ( 'NONE',  ( -0.02181900108494696719, 0.000000000000000000, 0.9997619372588931741 ) ) ;
#12422 = APPLICATION_CONTEXT ( 'configuration controlled 3d designs of mechanical parts and assemblies' ) ;
#12423 = EDGE_LOOP ( 'NONE', ( #13528, #12851, #12372, #5807 ) ) ;
#12424 = EDGE_CURVE ( 'NONE', #14484, #4505, #1630, .T. ) ;
#12425 = CIRCLE ( 'NONE', #5764, 3.500000000000003109 ) ;
#12426 = EDGE_CURVE ( 'NONE', #411, #15277, #2715, .T. ) ;
#12427 = DIRECTION ( 'NONE',  ( 0.000000000000000000, 1.000000000000000000, 0.000000000000000000 ) ) ;
#12428 = AXIS2_PLACEMENT_3D ( 'NONE', #12168, #3908, #1586 ) ;
#12429 = CARTESIAN_POINT ( 'NONE',  ( 3.249999999999998224, 4.187500000000000888, -4.846194077712561388 ) ) ;
#12430 = CARTESIAN_POINT ( 'NONE',  ( -3.249999999999999112, 11.68749999999999822, -2.153805922287440833 ) ) ;
#12431 = CARTESIAN_POINT ( 'NONE',  ( -4.050120478506952004, 15.00000000000000000, -103.2318605270664591 ) ) ;
#12432 = CYLINDRICAL_SURFACE ( 'NONE', #4540, 5.000000000000000000 ) ;
#12433 = CARTESIAN_POINT ( 'NONE',  ( -1.346194077712559389, 7.062500000000000000, -0.2500000000000002220 ) ) ;
#12434 = CARTESIAN_POINT ( 'NONE',  ( -3.750000000000000000, 6.812500000000000000, -5.053300858899105741 ) ) ;
#12435 = CARTESIAN_POINT ( 'NONE',  ( 3.749999999999999112, 9.687500000000000000, -5.053300858899108405 ) ) ;
#12436 = DIRECTION ( 'NONE',  ( 0.000000000000000000, 1.000000000000000000, 0.000000000000000000 ) ) ;
#12437 = EDGE_LOOP ( 'NONE', ( #15261, #2129, #3980, #3519 ) ) ;
#12438 = CARTESIAN_POINT ( 'NONE',  ( -3.803032749128815837, 10.37790251371667694, -43.21158422952260736 ) ) ;
#12439 = CARTESIAN_POINT ( 'NONE',  ( 2.651650429449552870, 10.12500000000000000, -6.151650429449555091 ) ) ;
#12440 = AXIS2_PLACEMENT_3D ( 'NONE', #14000, #6951, #9199 ) ;
#12441 = CARTESIAN_POINT ( 'NONE',  ( 3.136841903360915396, 9.999999999999998224, -104.4936450199714955 ) ) ;
#12442 = AXIS2_PLACEMENT_3D ( 'NONE', #5567, #13772, #7813 ) ;
#12443 = CC_DESIGN_PERSON_AND_ORGANIZATION_ASSIGNMENT ( #11475, #10309, ( #9134 ) ) ;
#12444 = LINE ( 'NONE', #14939, #1751 ) ;
#12445 = CARTESIAN_POINT ( 'NONE',  ( 13.10812892772005966, 2.100000000000000089, 17.79937169134660024 ) ) ;
#12446 = EDGE_CURVE ( 'NONE', #8293, #9274, #9128, .T. ) ;
#12447 = CARTESIAN_POINT ( 'NONE',  ( -26.92103615529513760, -3.820545969703583956E-12, -176.7902989741743625 ) ) ;
#12448 = CARTESIAN_POINT ( 'NONE',  ( 12.18103126625983812, 2.151585356863087384, -166.0646392245766663 ) ) ;
#12449 = EDGE_CURVE ( 'NONE', #2826, #5201, #11470, .T. ) ;
#12450 = CARTESIAN_POINT ( 'NONE',  ( -32.01906953552002477, 9.999999999999998224, -156.2419951537547718 ) ) ;
#12451 = ADVANCED_FACE ( 'NONE', ( #6269 ), #12886, .F. ) ;
#12452 = CARTESIAN_POINT ( 'NONE',  ( 1.553300858899109516, 14.43750000000000178, 0.2499999999999993616 ) ) ;
#12453 = EDGE_LOOP ( 'NONE', ( #2972, #10033, #2821, #8856, #11846 ) ) ;
#12454 = MANIFOLD_SOLID_BREP ( 'Cortar-Extruir2', #10786 ) ;
#12455 = CARTESIAN_POINT ( 'NONE',  ( 30.32986759126112730, 1.750000000000000000, 43.04214087805580391 ) ) ;
#12456 = CARTESIAN_POINT ( 'NONE',  ( 11.28543669177601494, 4.325399326098414043, -106.3987031433302377 ) ) ;
#12457 = CIRCLE ( 'NONE', #3556, 2.000000000000011546 ) ;
#12458 = DIRECTION ( 'NONE',  ( 0.000000000000000000, 0.000000000000000000, 1.000000000000000000 ) ) ;
#12459 = CARTESIAN_POINT ( 'NONE',  ( -3.980102097228897738E-16, 8.000000000000000000, -6.749999999999999112 ) ) ;
#12460 = CARTESIAN_POINT ( 'NONE',  ( 25.81993756863266398, 1.397373862231122054E-11, -140.3392227824482177 ) ) ;
#12461 = CARTESIAN_POINT ( 'NONE',  ( -3.749999999999999556, 13.18749999999999822, -1.946699141100892927 ) ) ;
#12462 = CARTESIAN_POINT ( 'NONE',  ( -68.68211634215907679, 9.999999999999998224, -201.9941738952850017 ) ) ;
#12463 = DIRECTION ( 'NONE',  ( -0.000000000000000000, 1.000000000000000000, -0.000000000000000000 ) ) ;
#12464 = CARTESIAN_POINT ( 'NONE',  ( -1.346194077712559389, 13.06250000000000000, -0.2500000000000002220 ) ) ;
#12465 = CARTESIAN_POINT ( 'NONE',  ( -0.3766621274091715987, 0.2004420829692335482, 0.1491815183709511161 ) ) ;
#12466 = DIRECTION ( 'NONE',  ( -0.000000000000000000, 1.000000000000000000, -0.000000000000000000 ) ) ;
#12467 = CARTESIAN_POINT ( 'NONE',  ( -3.249999999999999556, 8.187500000000000000, -2.153805922287440833 ) ) ;
#12468 = DIRECTION ( 'NONE',  ( -0.9961255586397056438, 0.000000000000000000, 0.08794243244722428632 ) ) ;
#12469 = CARTESIAN_POINT ( 'NONE',  ( 10.95232128968187091, 11.68831177261878373, -43.87656800833052984 ) ) ;
#12470 = ORIENTED_EDGE ( 'NONE', *, *, #2236, .T. ) ;
#12471 = DIRECTION ( 'NONE',  ( 1.000000000000000000, 0.000000000000000000, 0.000000000000000000 ) ) ;
#12472 = CARTESIAN_POINT ( 'NONE',  ( -23.68884049351463972, 3.999999999999999112, -206.7022962662250904 ) ) ;
#12473 = CARTESIAN_POINT ( 'NONE',  ( -3.750000000000000000, 0.2500000000000000555, -3.499999999999999112 ) ) ;
#12474 = CARTESIAN_POINT ( 'NONE',  ( 3.249999999999998224, 15.18750000000000355, -4.846194077712561388 ) ) ;
#12475 = CARTESIAN_POINT ( 'NONE',  ( -3.249999999999999556, 0.2500000000000000000, -3.499999999999999556 ) ) ;
#12476 = ORIENTED_EDGE ( 'NONE', *, *, #10940, .T. ) ;
#12477 = SHAPE_REPRESENTATION ( 'BladeScrew_Predeterminado', ( #9419 ), #6228 ) ;
#12478 = CARTESIAN_POINT ( 'NONE',  ( -3.249999999999999556, 9.250000000000000000, -3.499999999999999556 ) ) ;
#12479 = CARTESIAN_POINT ( 'NONE',  ( 10.04079546391108124, 11.77387431541663076, -44.82333900155087747 ) ) ;
#12480 = CARTESIAN_POINT ( 'NONE',  ( 10.56990542994451410, 15.00000000000000355, -125.5400580087990505 ) ) ;
#12481 = DIRECTION ( 'NONE',  ( 0.000000000000000000, 0.000000000000000000, 1.000000000000000000 ) ) ;
#12482 = CARTESIAN_POINT ( 'NONE',  ( -8.786545012121958820, 12.38245414974118930, -115.6253344005690877 ) ) ;
#12483 = COORDINATED_UNIVERSAL_TIME_OFFSET ( 0, 0, .AHEAD. ) ;
#12484 = CARTESIAN_POINT ( 'NONE',  ( 8.308576004177995245, 15.00000000000000000, -113.5907613746703220 ) ) ;
#12485 = CARTESIAN_POINT ( 'NONE',  ( 24.26046657763140857, 0.6944454239927166928, -138.1842452301896742 ) ) ;
#12486 = B_SPLINE_CURVE_WITH_KNOTS ( 'NONE', 3,
 ( #6804, #11738, #4345, #3169, #936, #7880, #10353, #15174, #15095, #4567 ),
 .UNSPECIFIED., .F., .F.,
 ( 4, 2, 2, 2, 4 ),
 ( 8.673617379884035472E-19, 0.009142429936519546468, 0.01828485987303909294, 0.02742728980955863941, 0.03656971974607818587 ),
 .UNSPECIFIED. ) ;
#12487 = VERTEX_POINT ( 'NONE', #1471 ) ;
#12488 = CARTESIAN_POINT ( 'NONE',  ( 3.249999999999999556, 4.750000000000000000, -3.500000000000000000 ) ) ;
#12489 = CARTESIAN_POINT ( 'NONE',  ( -2.837468109123414628, -2.075239479414269894, -0.7946808062269106188 ) ) ;
#12490 = CARTESIAN_POINT ( 'NONE',  ( -1.553300858899107073, 2.937500000000000444, -7.249999999999999112 ) ) ;
#12491 = VERTEX_POINT ( 'NONE', #7340 ) ;
#12492 = DIRECTION ( 'NONE',  ( 0.000000000000000000, 0.000000000000000000, -1.000000000000000000 ) ) ;
#12493 = DIRECTION ( 'NONE',  ( 0.000000000000000000, 0.000000000000000000, 1.000000000000000000 ) ) ;
#12494 = EDGE_CURVE ( 'NONE', #333, #6670, #6785, .T. ) ;
#12495 = CARTESIAN_POINT ( 'NONE',  ( 2.651650429449552870, 3.625000000000000000, -6.151650429449554203 ) ) ;
#12496 = CARTESIAN_POINT ( 'NONE',  ( 7.379366129813715425, 4.011723206745021031, -25.58330403907983097 ) ) ;
#12497 = CARTESIAN_POINT ( 'NONE',  ( 0.05436568487884790857, 2.499999997174701338, 0.6158011180084422831 ) ) ;
#12498 = CARTESIAN_POINT ( 'NONE',  ( -2.651650429449553314, 1.375000000000000000, -6.151650429449552426 ) ) ;
#12499 = COORDINATED_UNIVERSAL_TIME_OFFSET ( 0, 0, .AHEAD. ) ;
#12500 = CARTESIAN_POINT ( 'NONE',  ( -4.038200276543141953, 2.192442743657398552, -1.000000000000011768 ) ) ;
#12501 = ORIENTED_EDGE ( 'NONE', *, *, #6964, .F. ) ;
#12502 = CARTESIAN_POINT ( 'NONE',  ( 6.089666224640343017, 5.000000000000000000, -124.6062682140657074 ) ) ;
#12503 = CARTESIAN_POINT ( 'NONE',  ( -3.249999999999999112, 3.687500000000000444, -2.153805922287440833 ) ) ;
#12504 = CARTESIAN_POINT ( 'NONE',  ( 8.807773658247754156, 15.00000000000000000, -105.8689255569352667 ) ) ;
#12505 = CARTESIAN_POINT ( 'NONE',  ( -7.302595107033178046, 4.336808689942017736E-16, -125.2751219642074290 ) ) ;
#12506 = CARTESIAN_POINT ( 'NONE',  ( 2.651650429449553314, 4.375000000000000000, -0.8483495705504476847 ) ) ;
#12507 = CARTESIAN_POINT ( 'NONE',  ( -1.553300858899107073, 9.437500000000000000, -7.250000000000000000 ) ) ;
#12508 = AXIS2_PLACEMENT_3D ( 'NONE', #4871, #14479, #7263 ) ;
#12509 = ADVANCED_FACE ( 'NONE', ( #165 ), #6648, .T. ) ;
#12510 = DIRECTION ( 'NONE',  ( 0.000000000000000000, 0.000000000000000000, -1.000000000000000000 ) ) ;
#12511 = ORIENTED_EDGE ( 'NONE', *, *, #6406, .F. ) ;
#12512 = LINE ( 'NONE', #6793, #12366 ) ;
#12513 = CARTESIAN_POINT ( 'NONE',  ( 1.346194077712558057, 7.562500000000000000, -6.750000000000000000 ) ) ;
#12514 = CARTESIAN_POINT ( 'NONE',  ( 0.000000000000000000, 10.49999999999999822, 0.2500000000000002220 ) ) ;
#12515 = DIRECTION ( 'NONE',  ( -0.000000000000000000, -1.000000000000000000, -0.000000000000000000 ) ) ;
#12516 = CARTESIAN_POINT ( 'NONE',  ( 8.131300352726233527, -2.490287375297125294, -39.89901737624450107 ) ) ;
#12517 = CARTESIAN_POINT ( 'NONE',  ( 10.05869691007584521, 1.912799100046207235, -106.6366767720914623 ) ) ;
#12518 = ORIENTED_EDGE ( 'NONE', *, *, #7782, .F. ) ;
#12519 = CARTESIAN_POINT ( 'NONE',  ( -25.76048682929828004, 8.673617379884035472E-16, -193.9633714502515716 ) ) ;
#12520 = FACE_OUTER_BOUND ( 'NONE', #14866, .T. ) ;
#12521 = CARTESIAN_POINT ( 'NONE',  ( -42.91596092834496545, 15.00000000000000000, -158.7990843558665688 ) ) ;
#12522 = CARTESIAN_POINT ( 'NONE',  ( -3.249999999999999112, 3.812500000000000888, -4.846194077712558723 ) ) ;
#12523 = ORIENTED_EDGE ( 'NONE', *, *, #3847, .T. ) ;
#12524 = CARTESIAN_POINT ( 'NONE',  ( -1.500000000000000000, 4.500000000000000888, 0.2500000000000002220 ) ) ;
#12525 = CARTESIAN_POINT ( 'NONE',  ( 20.87131526946579285, 0.000000000000000000, -138.9752963459259547 ) ) ;
#12526 = CARTESIAN_POINT ( 'NONE',  ( -3.357927367646159844, 10.63007073917650125, -45.36065389210889975 ) ) ;
#12527 = CARTESIAN_POINT ( 'NONE',  ( 1.243260443319662123, 4.000000000000000000, -139.4020581015306846 ) ) ;
#12528 = CARTESIAN_POINT ( 'NONE',  ( -0.3214635616143260433, 5.000000000000000888, -103.0394908280558042 ) ) ;
#12529 = CARTESIAN_POINT ( 'NONE',  ( -3.249999999999999112, 9.812500000000000000, -4.846194077712558723 ) ) ;
#12530 = DESIGN_CONTEXT ( 'detailed design', #12731, 'design' ) ;
#12531 = EDGE_CURVE ( 'NONE', #3493, #6134, #121, .T. ) ;
#12532 = CARTESIAN_POINT ( 'NONE',  ( 22.79641070782754042, 8.673617379884035472E-16, -135.5653294067645049 ) ) ;
#12533 = CARTESIAN_POINT ( 'NONE',  ( -1.553300858899106629, 13.06250000000000000, 0.2500000000000002220 ) ) ;
#12534 = CARTESIAN_POINT ( 'NONE',  ( -67.56077634536279675, 14.99999999999568701, -204.5805788361718953 ) ) ;
#12535 = ADVANCED_FACE ( 'NONE', ( #8179 ), #5710, .F. ) ;
#12536 = ADVANCED_FACE ( 'NONE', ( #4482 ), #10304, .T. ) ;
#12537 = DIRECTION ( 'NONE',  ( -0.02181900108494732801, 0.000000000000000000, 0.9997619372588931741 ) ) ;
#12538 = CARTESIAN_POINT ( 'NONE',  ( 1.346194077712558057, 13.56250000000000000, -6.750000000000000000 ) ) ;
#12539 = DIRECTION ( 'NONE',  ( -8.673617379884027583E-16, 0.000000000000000000, -1.000000000000000000 ) ) ;
#12540 = DIRECTION ( 'NONE',  ( -0.9876883405951376593, 0.000000000000000000, 0.1564344650402315073 ) ) ;
#12541 = CARTESIAN_POINT ( 'NONE',  ( 3.249999999999998668, 8.687500000000000000, -4.846194077712560500 ) ) ;
#12542 = CARTESIAN_POINT ( 'NONE',  ( 2.759717552616797409, 0.1596090954753005553, 1.516153802207580670 ) ) ;
#12543 = CARTESIAN_POINT ( 'NONE',  ( 5.086353367585286556, 5.000000000000000888, -108.2668836821857639 ) ) ;
#12544 = B_SPLINE_CURVE_WITH_KNOTS ( 'NONE', 3,
 ( #15004, #9109, #13832, #2084, #11510, #926, #5626, #8551, #7314, #13287, #6155, #2690, #138, #64, #1376, #10724 ),
 .UNSPECIFIED., .F., .F.,
 ( 4, 2, 2, 2, 2, 2, 2, 4 ),
 ( 5.561946577567963334E-17, 0.0005014808200499583889, 0.001002961640099861050, 0.001504442460149763927, 0.002005923280199666588, 0.002507404100249569466, 0.003008884920299472344, 0.004011846560399272461 ),
 .UNSPECIFIED. ) ;
#12545 = VERTEX_POINT ( 'NONE', #13963 ) ;
#12546 = CARTESIAN_POINT ( 'NONE',  ( 8.966402098224863337, 12.25239120670691761, 1.441638956463255017 ) ) ;
#12547 = CARTESIAN_POINT ( 'NONE',  ( 4.018210755790066813, 15.00000000000000178, -105.8455740756232473 ) ) ;
#12548 = CARTESIAN_POINT ( 'NONE',  ( -2.651650429449552870, 1.125000000000000222, -0.8483495705504462414 ) ) ;
#12549 = CARTESIAN_POINT ( 'NONE',  ( -2.651650429449552870, 0.8750000000000000000, -6.151650429449552426 ) ) ;
#12550 = CARTESIAN_POINT ( 'NONE',  ( 1.346194077712558279, 14.06250000000000178, -6.750000000000000888 ) ) ;
#12551 = VERTEX_POINT ( 'NONE', #4374 ) ;
#12552 = CARTESIAN_POINT ( 'NONE',  ( 1.346194077712560944, 11.93750000000000000, -0.2500000000000010547 ) ) ;
#12553 = CARTESIAN_POINT ( 'NONE',  ( -3.249999999999999556, 11.31249999999999822, -4.846194077712557835 ) ) ;
#12554 = PLANE ( 'NONE',  #7912 ) ;
#12555 = EDGE_CURVE ( 'NONE', #14224, #12872, #8129, .T. ) ;
#12556 = CARTESIAN_POINT ( 'NONE',  ( -8.886921396801787054, 9.999999999999998224, -105.5168766094550250 ) ) ;
#12557 = CARTESIAN_POINT ( 'NONE',  ( -24.90112075662176139, 4.000000000000000888, -209.1976611213315493 ) ) ;
#12558 = CARTESIAN_POINT ( 'NONE',  ( -6.385995564644680655, 14.56253871825853530, -116.6487767744769712 ) ) ;
#12559 = PERSON_AND_ORGANIZATION_ROLE ( 'design_owner' ) ;
#12560 = CARTESIAN_POINT ( 'NONE',  ( 8.330271663372849744, 12.49999999999999822, -113.1592731357591788 ) ) ;
#12561 = CARTESIAN_POINT ( 'NONE',  ( -13.68460728451510455, 7.499999999999991118, -92.46488696946715891 ) ) ;
#12562 = CARTESIAN_POINT ( 'NONE',  ( 22.25559703696422531, 0.08303441296203807609, -138.6572023805229605 ) ) ;
#12563 = EDGE_LOOP ( 'NONE', ( #7502, #6944, #4602, #6356, #8386, #9296, #4999, #3662, #14196, #11982, #2466, #13615 ) ) ;
#12564 = CARTESIAN_POINT ( 'NONE',  ( 3.249999999999998668, 2.687500000000000888, -4.846194077712560500 ) ) ;
#12565 = DIRECTION ( 'NONE',  ( -0.9961255586397050887, -0.000000000000000000, 0.08794243244723005948 ) ) ;
#12566 =( BOUNDED_SURFACE ( )  B_SPLINE_SURFACE ( 3, 2, ( 
 ( #3811, #5963, #4886 ),
 ( #5882, #7277, #4814 ),
 ( #8207, #9598, #13081 ),
 ( #2496, #4965, #23 ),
 ( #4738, #14411, #9681 ),
 ( #14326, #2652, #7193 ),
 ( #9450, #7354, #10917 ),
 ( #12067, #6200, #5048 ),
 ( #3582, #13012, #11223 ),
 ( #8753, #14493, #1713 ),
 ( #13484, #1797, #14799 ),
 ( #13405, #8590, #2809 ),
 ( #1567, #11147, #12231 ),
 ( #1642, #7740, #6357 ),
 ( #566, #5276, #9987 ),
 ( #6582, #5497, #4493 ) ),
 .UNSPECIFIED., .F., .F., .F. ) 
 B_SPLINE_SURFACE_WITH_KNOTS ( ( 4, 2, 2, 2, 2, 2, 2, 4 ),
 ( 3, 3 ),
 ( -1.334638064063315278E-05, 0.001685485362004415181, 0.002534901233326939361, 0.003384317104649463542, 0.004233732975971987722, 0.005083148847294511469, 0.005932564718617035215, 0.006781980589939559829 ),
 ( 0.000000000000000000, 1.000000000000000000 ),
 .UNSPECIFIED. ) 
 GEOMETRIC_REPRESENTATION_ITEM ( )  RATIONAL_B_SPLINE_SURFACE ( (
 ( 1.000000000000000000, 1.000000000000000000, 1.000000000000000000),
 ( 1.000000000000000000, 0.9999849372739773035, 1.000000000000000000),
 ( 1.000000000000000000, 0.9937682810189589766, 1.000000000000000000),
 ( 1.000000000000000000, 0.9761755817002144564, 1.000000000000000000),
 ( 1.000000000000000000, 0.9688601978537728643, 1.000000000000000000),
 ( 1.000000000000000000, 0.9524575494629793360, 1.000000000000000000),
 ( 1.000000000000000000, 0.9433181971022835954, 1.000000000000000000),
 ( 1.000000000000000000, 0.9239129119538113111, 1.000000000000000000),
 ( 1.000000000000000000, 0.9135210720623375691, 1.000000000000000000),
 ( 1.000000000000000000, 0.8936014670382675940, 1.000000000000000000),
 ( 1.000000000000000000, 0.8840084896210586018, 1.000000000000000000),
 ( 1.000000000000000000, 0.8670987394481856070, 1.000000000000000000),
 ( 1.000000000000000000, 0.8600561105956274766, 1.000000000000000000),
 ( 1.000000000000000000, 0.8503557397563155096, 1.000000000000000000),
 ( 1.000000000000000000, 0.8476417977138580584, 1.000000000000000000),
 ( 1.000000000000000000, 0.8476602389438061547, 1.000000000000000000) ) ) 
 REPRESENTATION_ITEM ( '' )  SURFACE ( )  );
#12567 = CARTESIAN_POINT ( 'NONE',  ( -2.651650429449552870, 3.625000000000000888, -0.8483495705504463524 ) ) ;
#12568 = ORIENTED_EDGE ( 'NONE', *, *, #140, .T. ) ;
#12569 = CARTESIAN_POINT ( 'NONE',  ( -9.347739544678658419, 10.69911361329557486, -115.3723878648253702 ) ) ;
#12570 = CARTESIAN_POINT ( 'NONE',  ( 7.434948248173551377, 5.000000000000000888, -26.28946758364566705 ) ) ;
#12571 = CARTESIAN_POINT ( 'NONE',  ( 1.553300858899105963, 6.562500000000000000, -7.250000000000000888 ) ) ;
#12572 = LINE ( 'NONE', #10101, #15316 ) ;
#12573 = CARTESIAN_POINT ( 'NONE',  ( -3.762890103924136032, -1.083335593717819817E-30, -119.0450417366422755 ) ) ;
#12574 = CARTESIAN_POINT ( 'NONE',  ( -3.750000000000000000, 3.250000000000000444, -3.499999999999999112 ) ) ;
#12575 = PERSON_AND_ORGANIZATION_ROLE ( 'creator' ) ;
#12576 = DIRECTION ( 'NONE',  ( 0.000000000000000000, 0.000000000000000000, 1.000000000000000000 ) ) ;
#12577 = DIRECTION ( 'NONE',  ( -0.000000000000000000, 1.000000000000000000, -0.000000000000000000 ) ) ;
#12578 = LOCAL_TIME ( 12, 28, 20.00000000000000000, #12483 ) ;
#12579 = ORIENTED_EDGE ( 'NONE', *, *, #997, .F. ) ;
#12580 = CIRCLE ( 'NONE', #7886, 2.500000000000000000 ) ;
#12581 = CARTESIAN_POINT ( 'NONE',  ( 3.249999999999998224, 5.187499999999999112, -4.846194077712561388 ) ) ;
#12582 = CARTESIAN_POINT ( 'NONE',  ( -7.128555860240338049, 10.00000000000000000, -113.3867792963409471 ) ) ;
#12583 = CARTESIAN_POINT ( 'NONE',  ( 3.749999999999999556, 10.25000000000000178, -3.500000000000000444 ) ) ;
#12584 = CARTESIAN_POINT ( 'NONE',  ( 3.749999999999999112, 12.68750000000000178, -5.053300858899108405 ) ) ;
#12585 = SECURITY_CLASSIFICATION ( '', '', #13174 ) ;
#12586 = CARTESIAN_POINT ( 'NONE',  ( -8.031487215395415546, 1.587880349828493465, -115.9574366882091141 ) ) ;
#12587 = ORIENTED_EDGE ( 'NONE', *, *, #12923, .T. ) ;
#12588 = CARTESIAN_POINT ( 'NONE',  ( -3.897142427203911463, 10.21175642837406272, -43.91020597716068607 ) ) ;
#12589 = CARTESIAN_POINT ( 'NONE',  ( -3.980102097228897245E-16, 8.500000000000000000, -6.749999999999999112 ) ) ;
#12590 = CARTESIAN_POINT ( 'NONE',  ( -4.592425496802573972E-16, 8.999999999999998224, -7.250000000000000000 ) ) ;
#12591 = CARTESIAN_POINT ( 'NONE',  ( -4.601444581690889102, 4.336808689942017736E-16, -120.9301509763419205 ) ) ;
#12592 = PLANE ( 'NONE',  #6435 ) ;
#12593 = CARTESIAN_POINT ( 'NONE',  ( 9.939878312292615092, 15.00000000000000000, -115.2320631035898373 ) ) ;
#12594 = EDGE_LOOP ( 'NONE', ( #7189, #3051, #783, #11719, #14266, #10573, #11825, #13262, #12648, #15139 ) ) ;
#12595 = CARTESIAN_POINT ( 'NONE',  ( -29.76123416327401472, 2.196423649378339976E-12, -189.7991270702629834 ) ) ;
#12596 = CARTESIAN_POINT ( 'NONE',  ( 6.369258321017760238, -2.075239479414269894, -34.56909192082981974 ) ) ;
#12597 = CARTESIAN_POINT ( 'NONE',  ( -50.19288965985742834, 14.99999999999999467, -165.3052356887086773 ) ) ;
#12598 = LOCAL_TIME ( 12, 28, 20.00000000000000000, #11545 ) ;
#12599 = ADVANCED_FACE ( 'NONE', ( #11405 ), #1221, .T. ) ;
#12600 = CARTESIAN_POINT ( 'NONE',  ( -3.980102097228897738E-16, 3.000000000000000444, -6.749999999999999112 ) ) ;
#12601 = ORIENTED_EDGE ( 'NONE', *, *, #11927, .T. ) ;
#12602 = CARTESIAN_POINT ( 'NONE',  ( 1.667634992416483941, -2.570071824251322301, -1.000000000000001776 ) ) ;
#12603 = CARTESIAN_POINT ( 'NONE',  ( 7.995229681650334541, -1.921202954650395700, -34.56909192082981974 ) ) ;
#12604 = AXIS2_PLACEMENT_3D ( 'NONE', #11277, #7567, #8732 ) ;
#12605 = DIRECTION ( 'NONE',  ( -0.05964429961207245307, 0.000000000000000000, -0.9982196940171964572 ) ) ;
#12606 = AXIS2_PLACEMENT_3D ( 'NONE', #11955, #1216, #13130 ) ;
#12607 = CARTESIAN_POINT ( 'NONE',  ( 8.878875710790671505, 11.38038423757601691, 5.452159434543733418 ) ) ;
#12608 = CARTESIAN_POINT ( 'NONE',  ( 1.814459646442446061, 1.734723475976807094E-15, -110.3167319592340618 ) ) ;
#12609 = CARTESIAN_POINT ( 'NONE',  ( 3.249999999999998224, 10.31250000000000000, -2.153805922287439945 ) ) ;
#12610 = CARTESIAN_POINT ( 'NONE',  ( 17.61566365793502698, 8.673617379884035472E-16, -145.0049062421806809 ) ) ;
#12611 = CARTESIAN_POINT ( 'NONE',  ( -1.553300858899107295, 13.43749999999999822, -7.250000000000000000 ) ) ;
#12612 = DIRECTION ( 'NONE',  ( -0.000000000000000000, 0.000000000000000000, 1.000000000000000000 ) ) ;
#12613 = VECTOR ( 'NONE', #14696, 1000.000000000000000 ) ;
#12614 = CARTESIAN_POINT ( 'NONE',  ( 1.052436484934203387, 2.075239479414269894, -1.000000000000007772 ) ) ;
#12615 = CARTESIAN_POINT ( 'NONE',  ( 3.249999999999999112, 11.81249999999999822, -2.153805922287439945 ) ) ;
#12616 = AXIS2_PLACEMENT_3D ( 'NONE', #7175, #9355, #87 ) ;
#12617 = CARTESIAN_POINT ( 'NONE',  ( 0.5944212552585367293, 4.000000000000000000, -138.5540974747773930 ) ) ;
#12618 = CARTESIAN_POINT ( 'NONE',  ( 4.492499072540838689, 0.000000000000000000, -2.611025101989581820 ) ) ;
#12619 = CARTESIAN_POINT ( 'NONE',  ( -3.980102097228897245E-16, 7.500000000000000000, -6.749999999999999112 ) ) ;
#12620 = CARTESIAN_POINT ( 'NONE',  ( 11.44399236068192671, 6.000000000000000000, -138.9341978221715976 ) ) ;
#12621 = PLANE ( 'NONE',  #2963 ) ;
#12622 = ORIENTED_EDGE ( 'NONE', *, *, #14043, .F. ) ;
#12623 = EDGE_CURVE ( 'NONE', #10124, #2052, #10170, .T. ) ;
#12624 = ORIENTED_EDGE ( 'NONE', *, *, #9328, .T. ) ;
#12625 = CARTESIAN_POINT ( 'NONE',  ( -24.61436772009224327, 4.000000000000000000, -208.9121151917288728 ) ) ;
#12626 = CARTESIAN_POINT ( 'NONE',  ( -3.749999999999999556, 2.187500000000000444, -1.946699141100892927 ) ) ;
#12627 = CARTESIAN_POINT ( 'NONE',  ( 3.749999999999998668, 2.187500000000000000, -5.053300858899108405 ) ) ;
#12628 = EDGE_CURVE ( 'NONE', #13029, #14984, #1349, .T. ) ;
#12629 = CARTESIAN_POINT ( 'NONE',  ( -8.225432057702189326, -2.789143762251152850E-12, -106.0978137655278459 ) ) ;
#12630 = ORIENTED_EDGE ( 'NONE', *, *, #3712, .F. ) ;
#12631 = VECTOR ( 'NONE', #2, 1000.000000000000000 ) ;
#12632 = CARTESIAN_POINT ( 'NONE',  ( -2.298097038856278918, 9.375000000000000000, -5.798097038856277585 ) ) ;
#12633 = CARTESIAN_POINT ( 'NONE',  ( 10.95559245021438599, 11.70596818966908614, -43.87284672483780668 ) ) ;
#12634 = CARTESIAN_POINT ( 'NONE',  ( -8.105667775294676858, 13.14512866495358345, -104.3119030511063556 ) ) ;
#12635 = CARTESIAN_POINT ( 'NONE',  ( -7.490165920336979255, 13.90392860188294577, -116.1895725676876481 ) ) ;
#12636 = DATE_TIME_ROLE ( 'classification_date' ) ;
#12637 = CIRCLE ( 'NONE', #8687, 3.000000000000005329 ) ;
#12638 = CARTESIAN_POINT ( 'NONE',  ( 6.055984099849963442, 15.00000000000000000, -111.3700911571895347 ) ) ;
#12639 = DIRECTION ( 'NONE',  ( -0.1564344650402312298, -0.000000000000000000, 0.9876883405951376593 ) ) ;
#12640 = EDGE_LOOP ( 'NONE', ( #5607, #12511, #7469, #9089 ) ) ;
#12641 = CARTESIAN_POINT ( 'NONE',  ( 25.46731144555170090, 1.659276419459761565, -138.4193424522641180 ) ) ;
#12642 = CARTESIAN_POINT ( 'NONE',  ( 3.249999999999999112, 10.81250000000000178, -2.153805922287439945 ) ) ;
#12643 = ORIENTED_EDGE ( 'NONE', *, *, #555, .T. ) ;
#12644 = CARTESIAN_POINT ( 'NONE',  ( -1.346194077712559389, 6.437500000000000888, -6.749999999999999112 ) ) ;
#12645 = CARTESIAN_POINT ( 'NONE',  ( -3.578160823487106956, -2.490287375297124406, -0.5540151544739178036 ) ) ;
#12646 = CARTESIAN_POINT ( 'NONE',  ( 1.553300858899105963, 2.062500000000000000, -7.250000000000000888 ) ) ;
#12647 = ADVANCED_FACE ( 'NONE', ( #3593 ), #8294, .F. ) ;
#12648 = ORIENTED_EDGE ( 'NONE', *, *, #14349, .F. ) ;
#12649 = CARTESIAN_POINT ( 'NONE',  ( -1.242343264599803376, 7.379999999999995453, -42.49973277364670565 ) ) ;
#12650 = CARTESIAN_POINT ( 'NONE',  ( 3.249999999999998668, 0.6875000000000000000, -4.846194077712560500 ) ) ;
#12651 = AXIS2_PLACEMENT_3D ( 'NONE', #15005, #13413, #3236 ) ;
#12652 = CARTESIAN_POINT ( 'NONE',  ( 1.553300858899105963, 5.562500000000000000, -7.250000000000000888 ) ) ;
#12653 = CARTESIAN_POINT ( 'NONE',  ( -25.15392993456217852, 2.155093112943019751, -208.2125851377665242 ) ) ;
#12654 = DIRECTION ( 'NONE',  ( 0.02181900108494707821, 0.000000000000000000, -0.9997619372588931741 ) ) ;
#12655 = PERSON_AND_ORGANIZATION ( #3176, #3020 ) ;
#12656 = FACE_OUTER_BOUND ( 'NONE', #13439, .T. ) ;
#12657 =( BOUNDED_SURFACE ( )  B_SPLINE_SURFACE ( 3, 1, ( 
 ( #7927, #12489 ),
 ( #5677, #11486 ),
 ( #5381, #5531 ),
 ( #3208, #12645 ) ),
 .UNSPECIFIED., .F., .F., .F. ) 
 B_SPLINE_SURFACE_WITH_KNOTS ( ( 4, 4 ),
 ( 2, 2 ),
 ( 0.000000000000000000, 1.000000000000000000 ),
 ( 0.000000000000000000, 1.000000000000000000 ),
 .UNSPECIFIED. ) 
 GEOMETRIC_REPRESENTATION_ITEM ( )  RATIONAL_B_SPLINE_SURFACE ( (
 ( 1.000000000000000000, 1.000000000000000000),
 ( 0.6468719831415916666, 0.6468719831415916666),
 ( 0.6468719831415916666, 0.6468719831415916666),
 ( 1.000000000000000000, 1.000000000000000000) ) ) 
 REPRESENTATION_ITEM ( '' )  SURFACE ( )  );
#12658 = ORIENTED_EDGE ( 'NONE', *, *, #161, .F. ) ;
#12659 = CARTESIAN_POINT ( 'NONE',  ( -1.346194077712558945, 1.562500000000000222, -0.2500000000000002220 ) ) ;
#12660 = DIRECTION ( 'NONE',  ( 0.000000000000000000, 0.000000000000000000, 1.000000000000000000 ) ) ;
#12661 = CIRCLE ( 'NONE', #5751, 1.000000000000000888 ) ;
#12662 = CARTESIAN_POINT ( 'NONE',  ( -3.750000000000000000, 9.687500000000000000, -1.946699141100893149 ) ) ;
#12663 = CARTESIAN_POINT ( 'NONE',  ( -2.651650429449553314, 14.37500000000000000, -6.151650429449552426 ) ) ;
#12664 = CARTESIAN_POINT ( 'NONE',  ( -66.07114055912228423, 14.98244587632921387, -194.2582470785968383 ) ) ;
#12665 = CARTESIAN_POINT ( 'NONE',  ( -5.599106598294000925, 0.1460420930272973150, -117.2453520682029762 ) ) ;
#12666 = CARTESIAN_POINT ( 'NONE',  ( -1.346194077712558945, -0.4374999999999998890, -0.2500000000000002220 ) ) ;
#12667 = CARTESIAN_POINT ( 'NONE',  ( -5.753797509970949520, 4.336808689942017736E-16, -122.9860260041494229 ) ) ;
#12668 = DIRECTION ( 'NONE',  ( 1.000000000000000000, 0.000000000000000000, 0.000000000000000000 ) ) ;
#12669 = VECTOR ( 'NONE', #10914, 1000.000000000000000 ) ;
#12670 = DIRECTION ( 'NONE',  ( 0.000000000000000000, 0.000000000000000000, 1.000000000000000000 ) ) ;
#12671 = AXIS2_PLACEMENT_3D ( 'NONE', #13026, #10700, #5827 ) ;
#12672 = ORIENTED_EDGE ( 'NONE', *, *, #6168, .F. ) ;
#12673 = CARTESIAN_POINT ( 'NONE',  ( -29.01353551585973634, -1.091297840028627083E-12, -200.3078382963151398 ) ) ;
#12674 = CARTESIAN_POINT ( 'NONE',  ( -1.990360824022270991, 6.321094445766561876, -22.54485386122858515 ) ) ;
#12675 = CARTESIAN_POINT ( 'NONE',  ( -40.58904132556775579, 15.00000000000000000, -152.2044608390405074 ) ) ;
#12676 = CARTESIAN_POINT ( 'NONE',  ( 2.298097038856278029, 1.124999999999999778, -5.798097038856279362 ) ) ;
#12677 = VERTEX_POINT ( 'NONE', #2199 ) ;
#12678 = DIRECTION ( 'NONE',  ( 1.000000000000000000, 0.000000000000000000, 0.000000000000000000 ) ) ;
#12679 = LINE ( 'NONE', #4408, #318 ) ;
#12680 = DIRECTION ( 'NONE',  ( -0.000000000000000000, 1.000000000000000000, -0.000000000000000000 ) ) ;
#12681 = CARTESIAN_POINT ( 'NONE',  ( -2.298097038856278918, 10.37500000000000000, -5.798097038856277585 ) ) ;
#12682 = CARTESIAN_POINT ( 'NONE',  ( 51.19063959271458231, 0.000000000000000000, 70.12932606827693860 ) ) ;
#12683 = CARTESIAN_POINT ( 'NONE',  ( -3.768042520817070251, 5.000000000000000888, -109.5986228335811035 ) ) ;
#12684 = VECTOR ( 'NONE', #14533, 1000.000000000000000 ) ;
#12685 = CARTESIAN_POINT ( 'NONE',  ( 1.346194077712561166, 14.43750000000000178, -0.2500000000000011102 ) ) ;
#12686 = EDGE_CURVE ( 'NONE', #8123, #13993, #5310, .T. ) ;
#12687 = CARTESIAN_POINT ( 'NONE',  ( -4.348254188330000325, 7.379999999999995453, -49.25275560300654831 ) ) ;
#12688 = CARTESIAN_POINT ( 'NONE',  ( -4.592425496802573972E-16, 1.000000000000000000, -7.250000000000000000 ) ) ;
#12689 = ADVANCED_FACE ( 'NONE', ( #6052 ), #10545, .F. ) ;
#12690 = LINE ( 'NONE', #14162, #3490 ) ;
#12691 = CARTESIAN_POINT ( 'NONE',  ( 5.844703153020811115, 15.00000000000000000, -103.2023327213425432 ) ) ;
#12692 = CARTESIAN_POINT ( 'NONE',  ( 4.586756373948224663, 15.00000000000000178, -116.5615908754608228 ) ) ;
#12693 = CARTESIAN_POINT ( 'NONE',  ( 26.33833810415152143, 3.213311421644162724, -137.0172291339391961 ) ) ;
#12694 = CARTESIAN_POINT ( 'NONE',  ( 3.821260581353220331, 12.94577194562833533, 4.081242289023049530 ) ) ;
#12695 = CARTESIAN_POINT ( 'NONE',  ( -2.298097038856278473, 7.125000000000000000, -1.201902961143720416 ) ) ;
#12696 = AXIS2_PLACEMENT_3D ( 'NONE', #10560, #15296, #3528 ) ;
#12697 = CARTESIAN_POINT ( 'NONE',  ( 8.219148137521692377, 5.000000000000000888, -129.9861206050398721 ) ) ;
#12698 = DIRECTION ( 'NONE',  ( 0.000000000000000000, 0.000000000000000000, -1.000000000000000000 ) ) ;
#12699 = ORIENTED_EDGE ( 'NONE', *, *, #11119, .T. ) ;
#12700 = VERTEX_POINT ( 'NONE', #4600 ) ;
#12701 = FACE_OUTER_BOUND ( 'NONE', #11217, .T. ) ;
#12702 = CARTESIAN_POINT ( 'NONE',  ( -2.651650429449552870, 0.1250000000000000278, -0.8483495705504462414 ) ) ;
#12703 = CARTESIAN_POINT ( 'NONE',  ( 1.346194077712558279, 14.06250000000000178, -6.750000000000000888 ) ) ;
#12704 = CARTESIAN_POINT ( 'NONE',  ( -0.3733149413592447008, 15.00000000000000000, -108.7489923163346361 ) ) ;
#12705 = ORIENTED_EDGE ( 'NONE', *, *, #8181, .F. ) ;
#12706 = CARTESIAN_POINT ( 'NONE',  ( -3.249999999999999112, 0.8124999999999997780, -4.846194077712558723 ) ) ;
#12707 = EDGE_CURVE ( 'NONE', #11692, #9756, #12950, .T. ) ;
#12708 = VECTOR ( 'NONE', #1951, 1000.000000000000000 ) ;
#12709 = CARTESIAN_POINT ( 'NONE',  ( -5.581362024073984962, 5.000000000000000888, -111.7646305296507165 ) ) ;
#12710 = CARTESIAN_POINT ( 'NONE',  ( -8.738531072872435246, 12.15659329382392606, -104.5057571303798483 ) ) ;
#12711 = ADVANCED_FACE ( 'NONE', ( #2426 ), #11924, .F. ) ;
#12712 =( LENGTH_UNIT ( ) NAMED_UNIT ( * ) SI_UNIT ( .MILLI., .METRE. ) );
#12713 = CARTESIAN_POINT ( 'NONE',  ( 3.249999999999998668, 4.687500000000000888, -4.846194077712560500 ) ) ;
#12714 = DATE_AND_TIME ( #3588, #7141 ) ;
#12715 = CARTESIAN_POINT ( 'NONE',  ( 8.347943498206106483, 15.00000000000093614, -114.9028610997532382 ) ) ;
#12716 = CARTESIAN_POINT ( 'NONE',  ( 2.752881441477233349, 15.00000000000000000, 2.754251355355158637 ) ) ;
#12717 = VERTEX_POINT ( 'NONE', #3663 ) ;
#12718 = AXIS2_PLACEMENT_3D ( 'NONE', #13391, #1629, #11354 ) ;
#12719 = CARTESIAN_POINT ( 'NONE',  ( 21.58150087226717417, 1.257146728175858478E-15, -138.8928492084092454 ) ) ;
#12720 = CARTESIAN_POINT ( 'NONE',  ( -1.346194077712559167, 9.437500000000000000, -6.749999999999999112 ) ) ;
#12721 = EDGE_LOOP ( 'NONE', ( #10303, #7087, #13627, #4713 ) ) ;
#12722 = ORIENTED_EDGE ( 'NONE', *, *, #1088, .T. ) ;
#12723 = CARTESIAN_POINT ( 'NONE',  ( -2.651650429449552870, 8.624999999999998224, -0.8483495705504463524 ) ) ;
#12724 = DIRECTION ( 'NONE',  ( -0.000000000000000000, -1.000000000000000000, -0.000000000000000000 ) ) ;
#12725 = CARTESIAN_POINT ( 'NONE',  ( 0.000000000000000000, 0.5000000000000001110, 0.2500000000000002220 ) ) ;
#12726 = CARTESIAN_POINT ( 'NONE',  ( 1.346194077712558279, 5.062500000000000000, -6.750000000000000888 ) ) ;
#12727 = ORIENTED_EDGE ( 'NONE', *, *, #2408, .T. ) ;
#12728 = APPROVAL ( #364, 'UNSPECIFIED' ) ;
#12729 = CARTESIAN_POINT ( 'NONE',  ( -9.097645849187712130, 11.69616909788754811, -115.4858344565724906 ) ) ;
#12730 = CARTESIAN_POINT ( 'NONE',  ( -3.980102097228897245E-16, 2.500000000000000000, -6.749999999999999112 ) ) ;
#12731 = APPLICATION_CONTEXT ( 'configuration controlled 3d designs of mechanical parts and assemblies' ) ;
#12732 = CARTESIAN_POINT ( 'NONE',  ( -4.592425496802573972E-16, 5.500000000000000000, -7.249999999999999112 ) ) ;
#12733 = CARTESIAN_POINT ( 'NONE',  ( -24.72728013139317227, 3.011500147175719011, -208.3923052574565986 ) ) ;
#12734 = ADVANCED_FACE ( 'NONE', ( #7121 ), #7054, .T. ) ;
#12735 = CARTESIAN_POINT ( 'NONE',  ( -25.82983890416511841, 15.00000000000000000, -152.2527639562405000 ) ) ;
#12736 = EDGE_CURVE ( 'NONE', #6670, #6539, #3906, .T. ) ;
#12737 = CALENDAR_DATE ( 2026, 8, 10 ) ;
#12738 = EDGE_CURVE ( 'NONE', #5493, #7860, #5061, .T. ) ;
#12739 = CARTESIAN_POINT ( 'NONE',  ( 16.72930956226772992, 5.000000000000001776, -129.1652552991705249 ) ) ;
#12740 = DIRECTION ( 'NONE',  ( -0.9961255586397049777, -0.000000000000000000, 0.08794243244723005948 ) ) ;
#12741 = VERTEX_POINT ( 'NONE', #13336 ) ;
#12742 = CARTESIAN_POINT ( 'NONE',  ( -3.249999999999999112, 6.687500000000000888, -2.153805922287440833 ) ) ;
#12743 = CARTESIAN_POINT ( 'NONE',  ( 26.30339064689345463, 1.750000000000000000, 68.98786334397659914 ) ) ;
#12744 = CARTESIAN_POINT ( 'NONE',  ( 2.651650429449553314, 11.37500000000000178, -0.8483495705504476847 ) ) ;
#12745 = CARTESIAN_POINT ( 'NONE',  ( -2.651650429449552870, 14.12500000000000000, -0.8483495705504462414 ) ) ;
#12746 = CARTESIAN_POINT ( 'NONE',  ( -64.07341370074516362, 14.99999999999997691, -182.2352504702354565 ) ) ;
#12747 = ORIENTED_EDGE ( 'NONE', *, *, #56, .T. ) ;
#12748 = CARTESIAN_POINT ( 'NONE',  ( 0.000000000000000000, -0.2006112523677016091, 0.1491815183709511716 ) ) ;
#12749 = CARTESIAN_POINT ( 'NONE',  ( -1.553300858899106629, 13.56250000000000000, 0.2500000000000002220 ) ) ;
#12750 = CARTESIAN_POINT ( 'NONE',  ( 51.19063959271458231, 0.000000000000000000, 70.12932606827693860 ) ) ;
#12751 = PERSON_AND_ORGANIZATION_ROLE ( 'design_supplier' ) ;
#12752 = PRODUCT_RELATED_PRODUCT_CATEGORY ( 'detail', '', ( #8425 ) ) ;
#12753 = LINE ( 'NONE', #11659, #8480 ) ;
#12754 = ORIENTED_EDGE ( 'NONE', *, *, #9666, .T. ) ;
#12755 = CARTESIAN_POINT ( 'NONE',  ( 8.831196406527940468, 4.174746519320978067, 5.585086345355044557 ) ) ;
#12756 = CARTESIAN_POINT ( 'NONE',  ( 9.499156868358349826, 0.02433756043618112708, -163.5877548174848357 ) ) ;
#12757 = CARTESIAN_POINT ( 'NONE',  ( -57.99932148896577644, 15.00000000000000000, -167.8682911189483775 ) ) ;
#12758 = CARTESIAN_POINT ( 'NONE',  ( 3.249999999999998224, 3.187500000000000444, -4.846194077712561388 ) ) ;
#12759 = ORIENTED_EDGE ( 'NONE', *, *, #2781, .T. ) ;
#12760 = CARTESIAN_POINT ( 'NONE',  ( 10.01939027896081313, 5.000000000000000888, -127.6977514918621637 ) ) ;
#12761 = CARTESIAN_POINT ( 'NONE',  ( -25.67126045880329244, 1.369234990023930010, -206.3875020893990211 ) ) ;
#12762 = CIRCLE ( 'NONE', #5841, 3.250000000000003553 ) ;
#12763 = LINE ( 'NONE', #3479, #13178 ) ;
#12764 = CARTESIAN_POINT ( 'NONE',  ( 0.000000000000000000, 5.000000000000000888, -101.1952717268990369 ) ) ;
#12765 = CARTESIAN_POINT ( 'NONE',  ( -3.249999999999999112, 13.68750000000000178, -2.153805922287440833 ) ) ;
#12766 = LINE ( 'NONE', #8496, #7923 ) ;
#12767 = CARTESIAN_POINT ( 'NONE',  ( 3.749999999999999112, 2.187500000000000000, -5.053300858899108405 ) ) ;
#12768 = DIRECTION ( 'NONE',  ( 0.000000000000000000, 0.000000000000000000, -1.000000000000000000 ) ) ;
#12769 = CARTESIAN_POINT ( 'NONE',  ( 29.19009439915865656, 8.773889247172311556, -42.96359249924044832 ) ) ;
#12770 = B_SPLINE_CURVE_WITH_KNOTS ( 'NONE', 3,
 ( #5151, #8784, #1522, #13275, #7613, #2603, #7465, #6311, #6233, #8703, #366, #7303, #1670, #285, #1441, #12259, #5077, #10948 ),
 .UNSPECIFIED., .F., .F.,
 ( 4, 2, 2, 2, 2, 2, 2, 2, 4 ),
 ( -1.667338569123524410E-05, 0.002831516953986391253, 0.005679707293664017567, 0.007103802463502830074, 0.007815850048422199464, 0.008527897633341566253, 0.009951992803180237379, 0.01066404038809959896, 0.01137608797301896055 ),
 .UNSPECIFIED. ) ;
#12771 = VECTOR ( 'NONE', #5294, 1000.000000000000000 ) ;
#12772 = CARTESIAN_POINT ( 'NONE',  ( -11.55141596728015507, 9.999999999999996447, -126.4706876245357279 ) ) ;
#12773 = CARTESIAN_POINT ( 'NONE',  ( -3.384109865120556560, 0.000000000000000000, 30.80069534665370767 ) ) ;
#12774 = CARTESIAN_POINT ( 'NONE',  ( -3.249999999999999556, 7.312500000000000888, -4.846194077712557835 ) ) ;
#12775 = CARTESIAN_POINT ( 'NONE',  ( 2.862287955980151732, 14.99999999999999822, -24.43344328180646485 ) ) ;
#12776 = FACE_OUTER_BOUND ( 'NONE', #14911, .T. ) ;
#12777 = ORIENTED_EDGE ( 'NONE', *, *, #557, .T. ) ;
#12778 = ORIENTED_EDGE ( 'NONE', *, *, #12260, .T. ) ;
#12779 = CARTESIAN_POINT ( 'NONE',  ( -11.26695648740382971, 1.032514652406677416E-11, -186.6451589813374881 ) ) ;
#12780 = CARTESIAN_POINT ( 'NONE',  ( 1.553300858899108849, 6.937500000000000000, 0.2499999999999993616 ) ) ;
#12781 = CARTESIAN_POINT ( 'NONE',  ( -3.749999999999999556, 1.750000000000000000, -3.499999999999999112 ) ) ;
#12782 = CARTESIAN_POINT ( 'NONE',  ( 34.50563151437111742, 1.750000000003151257, 38.44810418511396222 ) ) ;
#12783 = EDGE_LOOP ( 'NONE', ( #2681, #7698, #12163, #9362, #5709, #9703, #6975, #13915, #3959, #3643 ) ) ;
#12784 = CARTESIAN_POINT ( 'NONE',  ( 1.346194077712558279, 2.062500000000000000, -6.750000000000000888 ) ) ;
#12785 = CARTESIAN_POINT ( 'NONE',  ( -2.298097038856278918, 11.37500000000000000, -5.798097038856277585 ) ) ;
#12786 = CARTESIAN_POINT ( 'NONE',  ( -57.71664061951929625, 9.999999999999998224, -153.6990377947290369 ) ) ;
#12787 = DIRECTION ( 'NONE',  ( 1.076984184057255515E-17, 1.000000000000000000, 1.219901976936984599E-16 ) ) ;
#12788 = CARTESIAN_POINT ( 'NONE',  ( 1.346194077712560944, 4.937500000000001776, -0.2500000000000010547 ) ) ;
#12789 = CARTESIAN_POINT ( 'NONE',  ( 8.961626804292983195, 15.00000000000000000, -105.6777632968436222 ) ) ;
#12790 = CARTESIAN_POINT ( 'NONE',  ( -9.108720832937514444, 12.32676068985322715, -116.5073105006875807 ) ) ;
#12791 = EDGE_LOOP ( 'NONE', ( #3467, #4603, #1502, #11462 ) ) ;
#12792 = CARTESIAN_POINT ( 'NONE',  ( -0.3766621274091715987, 0.5000000000000000000, -0.1347136637304948981 ) ) ;
#12793 = CARTESIAN_POINT ( 'NONE',  ( -1.346194077712559167, 10.43750000000000000, -6.749999999999999112 ) ) ;
#12794 = EDGE_CURVE ( 'NONE', #14561, #12868, #12000, .T. ) ;
#12795 = ORIENTED_EDGE ( 'NONE', *, *, #7064, .F. ) ;
#12796 = ORIENTED_EDGE ( 'NONE', *, *, #6013, .T. ) ;
#12797 = CARTESIAN_POINT ( 'NONE',  ( -3.750000000000000000, 10.68750000000000178, -1.946699141100893149 ) ) ;
#12798 = CARTESIAN_POINT ( 'NONE',  ( -1.160594694320683518, 2.331468351713110358E-16, 0.5210215923759189405 ) ) ;
#12799 = CARTESIAN_POINT ( 'NONE',  ( 0.000000000000000000, 1.500000000000000222, 0.2500000000000002220 ) ) ;
#12800 = CARTESIAN_POINT ( 'NONE',  ( 1.346194077712561166, 7.437500000000000000, -0.2500000000000011102 ) ) ;
#12801 = ORIENTED_EDGE ( 'NONE', *, *, #10884, .T. ) ;
#12802 = EDGE_CURVE ( 'NONE', #5040, #7422, #1725, .T. ) ;
#12803 = CARTESIAN_POINT ( 'NONE',  ( 8.673617379884035472E-16, 9.999999999999998224, -100.6237003951525537 ) ) ;
#12804 = CARTESIAN_POINT ( 'NONE',  ( -2.298097038856278473, 1.125000000000000222, -1.201902961143720416 ) ) ;
#12805 = CARTESIAN_POINT ( 'NONE',  ( 1.553300858899105963, 7.562500000000000000, -7.250000000000000888 ) ) ;
#12806 = CARTESIAN_POINT ( 'NONE',  ( -25.10588189737052645, 1.246347066797810932, -206.0870911841997497 ) ) ;
#12807 = DIRECTION ( 'NONE',  ( 0.9997619372588931741, 0.000000000000000000, 0.02181900108494707474 ) ) ;
#12808 = CC_DESIGN_PERSON_AND_ORGANIZATION_ASSIGNMENT ( #3855, #3773, ( #14121 ) ) ;
#12809 = DATE_AND_TIME ( #12737, #6408 ) ;
#12810 = CARTESIAN_POINT ( 'NONE',  ( -59.43466587753848529, 15.00000000000000000, -167.4626871265230648 ) ) ;
#12811 = DIRECTION ( 'NONE',  ( 0.000000000000000000, -1.000000000000000000, 0.000000000000000000 ) ) ;
#12812 = ORIENTED_EDGE ( 'NONE', *, *, #1681, .F. ) ;
#12813 = CARTESIAN_POINT ( 'NONE',  ( 2.298097038856278029, 6.125000000000000000, -5.798097038856279362 ) ) ;
#12814 = EDGE_CURVE ( 'NONE', #745, #1429, #5933, .T. ) ;
#12815 = CARTESIAN_POINT ( 'NONE',  ( 10.49113263805003982, 14.16484045804872061, -106.7936367227621730 ) ) ;
#12816 = ADVANCED_FACE ( 'NONE', ( #5214 ), #11616, .F. ) ;
#12817 = CARTESIAN_POINT ( 'NONE',  ( 0.000000000000000000, 9.500000000000001776, 0.2499999999999998057 ) ) ;
#12818 = CARTESIAN_POINT ( 'NONE',  ( -1.553300858899106407, 12.06250000000000000, 0.2500000000000002220 ) ) ;
#12819 = CARTESIAN_POINT ( 'NONE',  ( -65.23046657217157929, 14.71819778739303963, -193.2613010425793334 ) ) ;
#12820 = LINE ( 'NONE', #13987, #11862 ) ;
#12821 = CARTESIAN_POINT ( 'NONE',  ( 2.298097038856279362, 7.875000000000000000, -1.201902961143720860 ) ) ;
#12822 = CARTESIAN_POINT ( 'NONE',  ( 3.749999999999999112, 13.18750000000000000, -5.053300858899108405 ) ) ;
#12823 = CARTESIAN_POINT ( 'NONE',  ( -2.864308947300851838, 4.336808689942017243E-16, -115.9303594865754121 ) ) ;
#12824 = COORDINATED_UNIVERSAL_TIME_OFFSET ( 0, 0, .AHEAD. ) ;
#12825 = LINE ( 'NONE', #5559, #4815 ) ;
#12826 = ORIENTED_EDGE ( 'NONE', *, *, #14252, .T. ) ;
#12827 = CARTESIAN_POINT ( 'NONE',  ( -28.49016282317369431, 1.093032563504590562E-12, -202.0976090756554697 ) ) ;
#12828 = CARTESIAN_POINT ( 'NONE',  ( -3.980102097228897245E-16, 4.500000000000000888, -6.749999999999999112 ) ) ;
#12829 = CARTESIAN_POINT ( 'NONE',  ( -55.44729830678861049, 9.999999999999998224, -173.4678552873548654 ) ) ;
#12830 = CARTESIAN_POINT ( 'NONE',  ( 2.298097038856278029, 2.125000000000000000, -5.798097038856279362 ) ) ;
#12831 = EDGE_LOOP ( 'NONE', ( #2914, #10024, #15240 ) ) ;
#12832 = DIRECTION ( 'NONE',  ( 0.000000000000000000, 0.000000000000000000, -1.000000000000000000 ) ) ;
#12833 = EDGE_CURVE ( 'NONE', #2807, #6301, #515, .T. ) ;
#12834 = CARTESIAN_POINT ( 'NONE',  ( -3.520407287333055635, 7.379999999999995453, -45.56125597433126018 ) ) ;
#12835 = LOCAL_TIME ( 12, 28, 20.00000000000000000, #7706 ) ;
#12836 = CARTESIAN_POINT ( 'NONE',  ( 8.949236727333637731, 11.66009932332230647, 2.228168293400664357 ) ) ;
#12837 = CARTESIAN_POINT ( 'NONE',  ( -1.586855474365579610, 8.673617379884035472E-16, -114.8059160835070429 ) ) ;
#12838 = CARTESIAN_POINT ( 'NONE',  ( -3.249999999999999112, 12.81250000000000178, -4.846194077712558723 ) ) ;
#12839 = CIRCLE ( 'NONE', #5667, 3.000000000000010214 ) ;
#12840 = CARTESIAN_POINT ( 'NONE',  ( 4.624333745513746763, 8.673617379884034486E-16, -103.8844720882033812 ) ) ;
#12841 = CARTESIAN_POINT ( 'NONE',  ( -4.592425496802573972E-16, 2.000000000000000000, -7.250000000000000000 ) ) ;
#12842 = PLANE ( 'NONE',  #5031 ) ;
#12843 = CARTESIAN_POINT ( 'NONE',  ( 1.238244973495889356, 2.474488745542209767, -1.000000000000001332 ) ) ;
#12844 = CARTESIAN_POINT ( 'NONE',  ( 26.47489239128982419, 3.551309734749960256, -136.9665625843822170 ) ) ;
#12845 = CARTESIAN_POINT ( 'NONE',  ( -5.808150136390151097, 15.00000000000030020, -117.3161822536942793 ) ) ;
#12846 = CARTESIAN_POINT ( 'NONE',  ( 22.24275793208308016, 2.100000000000000089, 68.87427881220452264 ) ) ;
#12847 = CARTESIAN_POINT ( 'NONE',  ( -2.298097038856278918, 14.37500000000000000, -5.798097038856277585 ) ) ;
#12848 = VECTOR ( 'NONE', #15106, 1000.000000000000227 ) ;
#12849 = FACE_OUTER_BOUND ( 'NONE', #11313, .T. ) ;
#12850 = CARTESIAN_POINT ( 'NONE',  ( -3.545188519422978413, 10.00000000000000000, -132.7285785787237558 ) ) ;
#12851 = ORIENTED_EDGE ( 'NONE', *, *, #2158, .F. ) ;
#12852 = ORIENTED_EDGE ( 'NONE', *, *, #13032, .F. ) ;
#12853 = CARTESIAN_POINT ( 'NONE',  ( 9.899772909143624844, 12.50000000000000355, -108.5406452818202894 ) ) ;
#12854 = CARTESIAN_POINT ( 'NONE',  ( -2.651650429449553314, 3.375000000000000000, -6.151650429449552426 ) ) ;
#12855 = CARTESIAN_POINT ( 'NONE',  ( 0.000000000000000000, 3.500000000000000000, 0.2499999999999998057 ) ) ;
#12856 = CARTESIAN_POINT ( 'NONE',  ( -5.647163608656509126, 4.336808689942017736E-16, -105.1820076059687636 ) ) ;
#12857 = ORIENTED_EDGE ( 'NONE', *, *, #1384, .F. ) ;
#12858 = CARTESIAN_POINT ( 'NONE',  ( 2.298097038856278473, 14.62500000000000000, -5.798097038856279362 ) ) ;
#12859 = AXIS2_PLACEMENT_3D ( 'NONE', #9379, #8140, #14032 ) ;
#12860 = TOROIDAL_SURFACE ( 'NONE', #1991, 2.000000000000009326, 1.000000000000000000 ) ;
#12861 = CARTESIAN_POINT ( 'NONE',  ( -2.869987474717051068, -2.075239479414269894, -1.000000000000004441 ) ) ;
#12862 = VECTOR ( 'NONE', #3021, 1000.000000000000227 ) ;
#12863 = CARTESIAN_POINT ( 'NONE',  ( -8.886921396742344825, 10.34875921370766072, -105.5168766095049193 ) ) ;
#12864 = CARTESIAN_POINT ( 'NONE',  ( 2.298097038856279362, 4.875000000000000000, -1.201902961143720860 ) ) ;
#12865 = SECURITY_CLASSIFICATION_LEVEL ( 'unclassified' ) ;
#12866 = CARTESIAN_POINT ( 'NONE',  ( 10.54086443169194531, 14.99999999999764988, -107.6778029778606225 ) ) ;
#12867 = CARTESIAN_POINT ( 'NONE',  ( 10.87631271606135819, 1.290928924814131768E-12, -121.9832090784181275 ) ) ;
#12868 = VERTEX_POINT ( 'NONE', #7524 ) ;
#12869 = CARTESIAN_POINT ( 'NONE',  ( -1.760020797288979866, 14.99999999999999645, -120.7474935399611837 ) ) ;
#12870 = CARTESIAN_POINT ( 'NONE',  ( -2.298097038856278918, 12.37500000000000000, -5.798097038856277585 ) ) ;
#12871 = TOROIDAL_SURFACE ( 'NONE', #6932, 2.000000000000000000, 5.000000000000000000 ) ;
#12872 = VERTEX_POINT ( 'NONE', #4976 ) ;
#12873 = ORIENTED_EDGE ( 'NONE', *, *, #13703, .T. ) ;
#12874 = CARTESIAN_POINT ( 'NONE',  ( 0.000000000000000000, 9.500000000000000000, 0.2500000000000002220 ) ) ;
#12875 = DIRECTION ( 'NONE',  ( 0.02181900108494732801, 0.000000000000000000, -0.9997619372588931741 ) ) ;
#12876 = CARTESIAN_POINT ( 'NONE',  ( -3.749999999999999556, 4.750000000000000888, -3.499999999999999112 ) ) ;
#12877 = CARTESIAN_POINT ( 'NONE',  ( 0.000000000000000000, 7.500000000000000888, -0.2500000000000002220 ) ) ;
#12878 = ORIENTED_EDGE ( 'NONE', *, *, #2408, .F. ) ;
#12879 = DIRECTION ( 'NONE',  ( 0.7995711366325320979, 5.548139285719649595E-16, 0.6005713924789963798 ) ) ;
#12880 = CARTESIAN_POINT ( 'NONE',  ( 3.249999999999999556, 1.750000000000000000, -3.500000000000000000 ) ) ;
#12881 = PRODUCT ( 'PruningShears-Part2_Predeterminado', 'PruningShears-Part2_Predeterminado', '', ( #6067 ) ) ;
#12882 = CARTESIAN_POINT ( 'NONE',  ( -3.750000000000000000, 5.250000000000000000, -3.499999999999999112 ) ) ;
#12883 = AXIS2_PLACEMENT_3D ( 'NONE', #8461, #12093, #12012 ) ;
#12884 = CARTESIAN_POINT ( 'NONE',  ( -24.69689105420345143, 3.216921006046159270, -208.5365831628258206 ) ) ;
#12885 = CARTESIAN_POINT ( 'NONE',  ( 2.869574948089113509, -4.336808689942016947E-15, -131.9358007310388530 ) ) ;
#12886 =( BOUNDED_SURFACE ( )  B_SPLINE_SURFACE ( 3, 1, ( 
 ( #3713, #11979 ),
 ( #6345, #13153 ),
 ( #14397, #6026 ),
 ( #3952, #13067 ) ),
 .UNSPECIFIED., .F., .F., .T. ) 
 B_SPLINE_SURFACE_WITH_KNOTS ( ( 4, 4 ),
 ( 2, 2 ),
 ( 0.000000000000000000, 1.000000000000000000 ),
 ( 0.000000000000000000, 1.000000000000000000 ),
 .UNSPECIFIED. ) 
 GEOMETRIC_REPRESENTATION_ITEM ( )  RATIONAL_B_SPLINE_SURFACE ( (
 ( 1.000000000000000000, 1.000000000000000000),
 ( 0.9999990904828330862, 0.9999990904828330862),
 ( 0.9999990904828330862, 0.9999990904828330862),
 ( 1.000000000000000000, 1.000000000000000000) ) ) 
 REPRESENTATION_ITEM ( '' )  SURFACE ( )  );
#12887 = FACE_OUTER_BOUND ( 'NONE', #7773, .T. ) ;
#12888 = CALENDAR_DATE ( 2026, 8, 10 ) ;
#12889 = ADVANCED_FACE ( 'NONE', ( #12243 ), #1003, .T. ) ;
#12890 = CARTESIAN_POINT ( 'NONE',  ( -54.80563802043110400, 15.00000000000000178, -158.4804275959015172 ) ) ;
#12891 = ORIENTED_EDGE ( 'NONE', *, *, #14636, .T. ) ;
#12892 = CARTESIAN_POINT ( 'NONE',  ( -3.249999999999999112, 8.687500000000003553, -2.153805922287440833 ) ) ;
#12893 =( GEOMETRIC_REPRESENTATION_CONTEXT ( 3 ) GLOBAL_UNCERTAINTY_ASSIGNED_CONTEXT ( ( #11137 ) ) GLOBAL_UNIT_ASSIGNED_CONTEXT ( ( #1419, #5967, #7197 ) ) REPRESENTATION_CONTEXT ( 'NONE', 'WORKASPACE' ) );
#12894 = CARTESIAN_POINT ( 'NONE',  ( 8.978461304436878621, 1.921202954650395478, -40.45944830867332342 ) ) ;
#12895 = CARTESIAN_POINT ( 'NONE',  ( -2.651650429449552870, 9.624999999999998224, -0.8483495705504467965 ) ) ;
#12896 = CARTESIAN_POINT ( 'NONE',  ( -3.750000000000000000, 14.31250000000000000, -5.053300858899105741 ) ) ;
#12897 = CARTESIAN_POINT ( 'NONE',  ( -67.61879412477036055, 13.23091809662344964, -201.4429213360547521 ) ) ;
#12898 = DIRECTION ( 'NONE',  ( 0.05964429961207246000, -0.000000000000000000, 0.9982196940171965682 ) ) ;
#12899 = CARTESIAN_POINT ( 'NONE',  ( -2.298097038856279362, -0.1249999999999999029, -5.798097038856278473 ) ) ;
#12900 = CARTESIAN_POINT ( 'NONE',  ( -9.651007058052471166, -2.046300565911432839E-31, -128.1008536839752878 ) ) ;
#12901 = DATE_AND_TIME ( #5783, #3263 ) ;
#12902 = EDGE_CURVE ( 'NONE', #1425, #15209, #3903, .T. ) ;
#12903 = CARTESIAN_POINT ( 'NONE',  ( 10.97171279554003043, 8.773889247172311556, -44.61149169061435060 ) ) ;
#12904 = ORIENTED_EDGE ( 'NONE', *, *, #2433, .T. ) ;
#12905 = CARTESIAN_POINT ( 'NONE',  ( 6.122889822326360587, 4.740853562741660809, 5.281130613318502753 ) ) ;
#12906 = CARTESIAN_POINT ( 'NONE',  ( 1.346194077712560944, 4.937500000000000888, -0.2500000000000011102 ) ) ;
#12907 = CARTESIAN_POINT ( 'NONE',  ( -61.97126637942644578, 9.999999999999998224, -193.9440536785060374 ) ) ;
#12908 = CARTESIAN_POINT ( 'NONE',  ( -3.980102097228897738E-16, 6.000000000000000888, -6.749999999999999112 ) ) ;
#12909 = VERTEX_POINT ( 'NONE', #6293 ) ;
#12910 = CARTESIAN_POINT ( 'NONE',  ( -2.208383803796207356, 15.00000000000000000, -121.8037055012923986 ) ) ;
#12911 = B_SPLINE_CURVE_WITH_KNOTS ( 'NONE', 3,
 ( #260, #11301, #10071, #12465 ),
 .UNSPECIFIED., .F., .F.,
 ( 4, 4 ),
 ( 0.000000000000000000, 0.0003029267606473190228 ),
 .UNSPECIFIED. ) ;
#12912 = CARTESIAN_POINT ( 'NONE',  ( -25.20396192594209595, 0.003535883027464600988, -199.4400073539133871 ) ) ;
#12913 = CARTESIAN_POINT ( 'NONE',  ( 8.946924470861457479, 11.53290492750693197, 2.334117507164750638 ) ) ;
#12914 = CARTESIAN_POINT ( 'NONE',  ( 3.249999999999999556, 0.7500000000000000000, -3.500000000000000000 ) ) ;
#12915 = CARTESIAN_POINT ( 'NONE',  ( 1.346194077712558279, 14.06250000000000178, -6.750000000000000888 ) ) ;
#12916 = APPROVAL ( #13882, 'UNKNOWN' ) ;
#12917 = CARTESIAN_POINT ( 'NONE',  ( 4.917302814907795749, 8.673617379884035472E-16, -102.2758535390863273 ) ) ;
#12918 = CARTESIAN_POINT ( 'NONE',  ( 1.553300858899109516, 3.437500000000000444, 0.2499999999999993616 ) ) ;
#12919 = CIRCLE ( 'NONE', #4767, 10.00000000000000888 ) ;
#12920 = CARTESIAN_POINT ( 'NONE',  ( -25.82983890416511841, 15.00000000000000000, -157.2527639562405000 ) ) ;
#12921 = FACE_OUTER_BOUND ( 'NONE', #7319, .T. ) ;
#12922 = EDGE_CURVE ( 'NONE', #10207, #13643, #12352, .T. ) ;
#12923 = EDGE_CURVE ( 'NONE', #6272, #1043, #1580, .T. ) ;
#12924 = CARTESIAN_POINT ( 'NONE',  ( 24.49199709446414275, 1.068333355338896729, -137.6936497164150524 ) ) ;
#12925 = EDGE_CURVE ( 'NONE', #8581, #9140, #11375, .T. ) ;
#12926 = CARTESIAN_POINT ( 'NONE',  ( 4.869735923794943133, 0.000000000000000000, 48.16793894843318924 ) ) ;
#12927 = CARTESIAN_POINT ( 'NONE',  ( 3.249999999999999112, 11.81249999999999822, -2.153805922287439945 ) ) ;
#12928 = CARTESIAN_POINT ( 'NONE',  ( -8.134741379327362409, 13.10967652946907336, -104.3206942789991274 ) ) ;
#12929 = CARTESIAN_POINT ( 'NONE',  ( -64.12212600112349037, 13.16643233163841487, -201.2225177097709263 ) ) ;
#12930 = ORIENTED_EDGE ( 'NONE', *, *, #8286, .F. ) ;
#12931 = EDGE_LOOP ( 'NONE', ( #6708, #12601, #6766, #8604 ) ) ;
#12932 = CARTESIAN_POINT ( 'NONE',  ( 26.15341798802279527, 4.000000000000000000, -138.2600702976168350 ) ) ;
#12933 = CARTESIAN_POINT ( 'NONE',  ( 1.553300858899108849, 3.937500000000000000, 0.2499999999999993616 ) ) ;
#12934 = AXIS2_PLACEMENT_3D ( 'NONE', #4718, #12041, #8261 ) ;
#12935 = CARTESIAN_POINT ( 'NONE',  ( 3.749999999999998668, 6.187500000000001776, -5.053300858899108405 ) ) ;
#12936 = AXIS2_PLACEMENT_3D ( 'NONE', #14115, #116, #9241 ) ;
#12937 = CARTESIAN_POINT ( 'NONE',  ( 13.05714099816148277, 4.000000000000000000, -166.3497942184958447 ) ) ;
#12938 = EDGE_LOOP ( 'NONE', ( #8527, #11421, #4381, #203 ) ) ;
#12939 = B_SPLINE_CURVE_WITH_KNOTS ( 'NONE', 3,
 ( #9440, #2405, #15110, #14168 ),
 .UNSPECIFIED., .F., .F.,
 ( 4, 4 ),
 ( 0.000000000000000000, 0.03019882497682960937 ),
 .UNSPECIFIED. ) ;
#12940 = CARTESIAN_POINT ( 'NONE',  ( 0.000000000000000000, 1.500000000000000222, -0.2500000000000002220 ) ) ;
#12941 = CARTESIAN_POINT ( 'NONE',  ( -3.664341105599659976, 5.000000000000000000, -109.4598404583043703 ) ) ;
#12942 = DIRECTION ( 'NONE',  ( 0.08794243244723004560, 0.000000000000000000, 0.9961255586397049777 ) ) ;
#12943 = DIRECTION ( 'NONE',  ( 1.000000000000000000, 0.000000000000000000, 0.000000000000000000 ) ) ;
#12944 = CARTESIAN_POINT ( 'NONE',  ( -1.346194077712559389, 4.062500000000000000, -0.2500000000000002220 ) ) ;
#12945 = CIRCLE ( 'NONE', #1594, 1.000000000000000888 ) ;
#12946 = DATE_AND_TIME ( #11622, #507 ) ;
#12947 = CARTESIAN_POINT ( 'NONE',  ( -49.91314714375069173, 15.00000000000000000, -125.9106517931341500 ) ) ;
#12948 = CARTESIAN_POINT ( 'NONE',  ( 26.93149290009008823, 5.000000000000000888, -137.0203993314533761 ) ) ;
#12949 = ORIENTED_EDGE ( 'NONE', *, *, #13590, .F. ) ;
#12950 = LINE ( 'NONE', #12792, #274 ) ;
#12951 = FACE_OUTER_BOUND ( 'NONE', #12173, .T. ) ;
#12952 = VERTEX_POINT ( 'NONE', #347 ) ;
#12953 = ORIENTED_EDGE ( 'NONE', *, *, #8680, .T. ) ;
#12954 = CARTESIAN_POINT ( 'NONE',  ( -4.373225680752619304, 2.331468351711999543E-16, 27.28944397070847927 ) ) ;
#12955 = CARTESIAN_POINT ( 'NONE',  ( 2.651650429449552870, 5.125000000000000888, -6.151650429449555091 ) ) ;
#12956 = CARTESIAN_POINT ( 'NONE',  ( 1.346194077712558279, 8.062500000000001776, -6.750000000000000888 ) ) ;
#12957 = ORIENTED_EDGE ( 'NONE', *, *, #2627, .F. ) ;
#12958 = CARTESIAN_POINT ( 'NONE',  ( -0.06526978514036563261, 9.999999999999998224, -101.7940732946927227 ) ) ;
#12959 = CARTESIAN_POINT ( 'NONE',  ( 3.249999999999998668, 3.687500000000000444, -4.846194077712560500 ) ) ;
#12960 = CARTESIAN_POINT ( 'NONE',  ( -3.749999999999999556, 9.187500000000000000, -1.946699141100892927 ) ) ;
#12961 = CARTESIAN_POINT ( 'NONE',  ( -9.365519517993458720, 9.999999999999998224, -117.8403265034297505 ) ) ;
#12962 = DIRECTION ( 'NONE',  ( 0.000000000000000000, -1.000000000000000000, 0.000000000000000000 ) ) ;
#12963 = CARTESIAN_POINT ( 'NONE',  ( -9.742503157198443731, -2.490287375297125294, -40.35209559314896666 ) ) ;
#12964 = DATE_TIME_ROLE ( 'creation_date' ) ;
#12965 = B_SPLINE_CURVE_WITH_KNOTS ( 'NONE', 3,
 ( #13575, #8925, #6534, #13654, #510, #11169, #2758, #6306, #9937, #3054 ),
 .UNSPECIFIED., .F., .F.,
 ( 4, 2, 2, 2, 4 ),
 ( 1.430489624538199204E-17, 0.0007393650634207661089, 0.001478730126841517906, 0.002218095190262269704, 0.002957460253683021501 ),
 .UNSPECIFIED. ) ;
#12966 = LINE ( 'NONE', #2446, #12208 ) ;
#12967 = ORIENTED_EDGE ( 'NONE', *, *, #13094, .T. ) ;
#12968 = CARTESIAN_POINT ( 'NONE',  ( -2.298097038856278029, 8.625000000000000000, -1.201902961143720638 ) ) ;
#12969 = ADVANCED_FACE ( 'NONE', ( #497 ), #10846, .F. ) ;
#12970 = CARTESIAN_POINT ( 'NONE',  ( 9.458437899194636955, 0.000000000000000000, -40.77697206847473410 ) ) ;
#12971 = CARTESIAN_POINT ( 'NONE',  ( 0.000000000000000000, 11.50000000000000000, 0.2499999999999998057 ) ) ;
#12972 = CARTESIAN_POINT ( 'NONE',  ( 0.3766621274091715987, 0.5000000000000000000, 0.1491815183709511716 ) ) ;
#12973 = CARTESIAN_POINT ( 'NONE',  ( -64.70583122420893574, 13.98401442962929586, -198.8283618626409179 ) ) ;
#12974 = FACE_OUTER_BOUND ( 'NONE', #1633, .T. ) ;
#12975 = CARTESIAN_POINT ( 'NONE',  ( 3.249999999999998224, 0.3125000000000002220, -2.153805922287439945 ) ) ;
#12976 = CARTESIAN_POINT ( 'NONE',  ( 7.558695724227160184, 0.1516696207343164460, -105.3410990411258013 ) ) ;
#12977 = CALENDAR_DATE ( 2026, 8, 10 ) ;
#12978 = CARTESIAN_POINT ( 'NONE',  ( -1.376260179405567108, 15.00000000000000000, -106.6458321843530683 ) ) ;
#12979 = LINE ( 'NONE', #6003, #9892 ) ;
#12980 = VERTEX_POINT ( 'NONE', #577 ) ;
#12981 = CARTESIAN_POINT ( 'NONE',  ( -21.49135656595054655, 0.000000000000000000, -206.0886596525522236 ) ) ;
#12982 = CARTESIAN_POINT ( 'NONE',  ( -2.298097038856278918, 4.375000000000000000, -5.798097038856277585 ) ) ;
#12983 = CARTESIAN_POINT ( 'NONE',  ( -6.984815280171007501, 2.369024761733573552E-09, -104.2451759018677251 ) ) ;
#12984 = CARTESIAN_POINT ( 'NONE',  ( 1.346194077712558279, 6.062500000000000888, -6.750000000000000888 ) ) ;
#12985 = VERTEX_POINT ( 'NONE', #6214 ) ;
#12986 = CARTESIAN_POINT ( 'NONE',  ( -2.113448244030541989, 15.00000000000000000, -105.7248292520770008 ) ) ;
#12987 = DIRECTION ( 'NONE',  ( 0.08794243244722413366, 0.000000000000000000, 0.9961255586397056438 ) ) ;
#12988 = B_SPLINE_CURVE_WITH_KNOTS ( 'NONE', 1,
 ( #6669, #7897 ),
 .UNSPECIFIED., .F., .F.,
 ( 2, 2 ),
 ( 0.000000000000000000, 1.000000000000000000 ),
 .UNSPECIFIED. ) ;
#12989 = CARTESIAN_POINT ( 'NONE',  ( 6.089666224640342129, 15.00000000000000000, -124.6062682140657216 ) ) ;
#12990 = EDGE_CURVE ( 'NONE', #5891, #12700, #10929, .T. ) ;
#12991 = CARTESIAN_POINT ( 'NONE',  ( -1.346194077712559389, 0.06250000000000000000, -0.2500000000000002220 ) ) ;
#12992 = CARTESIAN_POINT ( 'NONE',  ( -3.249999999999999112, 14.81250000000000355, -4.846194077712558723 ) ) ;
#12993 = CARTESIAN_POINT ( 'NONE',  ( -3.750000000000000000, 4.312500000000000888, -5.053300858899105741 ) ) ;
#12994 = DIRECTION ( 'NONE',  ( 0.000000000000000000, 0.000000000000000000, 1.000000000000000000 ) ) ;
#12995 = CARTESIAN_POINT ( 'NONE',  ( -3.750000000000000000, 3.812500000000000888, -5.053300858899105741 ) ) ;
#12996 = CARTESIAN_POINT ( 'NONE',  ( -10.84779165590732752, 4.999999999999999112, -149.7094178749453590 ) ) ;
#12997 = CARTESIAN_POINT ( 'NONE',  ( -28.38930394846588001, 9.999999999999998224, -151.9126338648069066 ) ) ;
#12998 = LINE ( 'NONE', #2713, #4911 ) ;
#12999 = CARTESIAN_POINT ( 'NONE',  ( 20.23335552821398409, 0.000000000000000000, 65.44177069175029260 ) ) ;
#13000 = CARTESIAN_POINT ( 'NONE',  ( -3.249999999999999556, 11.31249999999999822, -4.846194077712557835 ) ) ;
#13001 = CARTESIAN_POINT ( 'NONE',  ( -7.917878791739701327, 13.35826822666819425, -104.2553089158425905 ) ) ;
#13002 = CARTESIAN_POINT ( 'NONE',  ( -64.17593475674455306, 14.99370959519457536, -182.8799376562455450 ) ) ;
#13003 = ORIENTED_EDGE ( 'NONE', *, *, #9009, .F. ) ;
#13004 = ORIENTED_EDGE ( 'NONE', *, *, #15009, .T. ) ;
#13005 = CARTESIAN_POINT ( 'NONE',  ( -2.612926366062044981, 4.336808689942017736E-16, -113.5913750124458801 ) ) ;
#13006 = CARTESIAN_POINT ( 'NONE',  ( -10.45827128286561702, 2.442921369471867893E-15, -185.7209244056693649 ) ) ;
#13007 = CARTESIAN_POINT ( 'NONE',  ( -2.651650429449552870, 4.125000000000000000, -0.8483495705504462414 ) ) ;
#13008 = CARTESIAN_POINT ( 'NONE',  ( -2.651650429449552870, 2.875000000000000000, -6.151650429449552426 ) ) ;
#13009 = DIRECTION ( 'NONE',  ( -0.000000000000000000, -1.000000000000000000, -0.000000000000000000 ) ) ;
#13010 = ORIENTED_EDGE ( 'NONE', *, *, #2677, .T. ) ;
#13011 = ADVANCED_FACE ( 'NONE', ( #5134 ), #10872, .T. ) ;
#13012 = CARTESIAN_POINT ( 'NONE',  ( -8.456080320763129876, 1.656510688599710290, -116.2291922150375001 ) ) ;
#13013 = CARTESIAN_POINT ( 'NONE',  ( 3.249999999999999556, 13.75000000000000000, -3.500000000000000000 ) ) ;
#13014 = EDGE_CURVE ( 'NONE', #5472, #7799, #14658, .T. ) ;
#13015 = CARTESIAN_POINT ( 'NONE',  ( -45.22661540093461952, 15.00000000000000000, -146.2291324070019982 ) ) ;
#13016 = PLANE ( 'NONE',  #10869 ) ;
#13017 = CARTESIAN_POINT ( 'NONE',  ( -6.938893903907228378E-15, 5.781808091008227457, -138.5079647995998471 ) ) ;
#13018 = CARTESIAN_POINT ( 'NONE',  ( 1.346194077712558057, 3.562500000000000444, -6.750000000000000000 ) ) ;
#13019 = PLANE ( 'NONE',  #5301 ) ;
#13020 = CARTESIAN_POINT ( 'NONE',  ( 21.65409573407107402, 8.673617379884035472E-16, -133.3516700272784590 ) ) ;
#13021 = EDGE_LOOP ( 'NONE', ( #10191, #4669, #10177, #6969 ) ) ;
#13022 = DIRECTION ( 'NONE',  ( 0.000000000000000000, 0.000000000000000000, -1.000000000000000000 ) ) ;
#13023 = CARTESIAN_POINT ( 'NONE',  ( 3.249999999999998668, 14.68750000000000178, -4.846194077712560500 ) ) ;
#13024 = ORIENTED_EDGE ( 'NONE', *, *, #3760, .T. ) ;
#13025 = ORIENTED_EDGE ( 'NONE', *, *, #13593, .T. ) ;
#13026 = CARTESIAN_POINT ( 'NONE',  ( -25.82983890416511841, 15.00000000000000000, -142.4527639562402328 ) ) ;
#13027 = CARTESIAN_POINT ( 'NONE',  ( 1.553300858899109516, 6.437500000000000888, 0.2499999999999993616 ) ) ;
#13028 = CARTESIAN_POINT ( 'NONE',  ( -2.298097038856278029, 4.625000000000000888, -1.201902961143720638 ) ) ;
#13029 = VERTEX_POINT ( 'NONE', #11157 ) ;
#13030 = CARTESIAN_POINT ( 'NONE',  ( 8.673617379884035472E-16, 9.999999999999998224, -101.1952717268916757 ) ) ;
#13031 = CARTESIAN_POINT ( 'NONE',  ( 3.249999999999999556, 2.750000000000000000, -3.500000000000000000 ) ) ;
#13032 = EDGE_CURVE ( 'NONE', #1429, #7022, #3471, .T. ) ;
#13033 = CARTESIAN_POINT ( 'NONE',  ( -5.402767302556228834, 2.500000000000000000, -110.8935206225344388 ) ) ;
#13034 = CARTESIAN_POINT ( 'NONE',  ( -38.89145998711707364, 9.999999999999998224, -156.9532850668581716 ) ) ;
#13035 = CARTESIAN_POINT ( 'NONE',  ( 9.200550766085388688, 14.99999999999999822, -124.0431718307209508 ) ) ;
#13036 = CALENDAR_DATE ( 2026, 8, 10 ) ;
#13037 = CARTESIAN_POINT ( 'NONE',  ( 3.158384440324535802, 0.2459835157955773399, -1.000000000000001110 ) ) ;
#13038 = VERTEX_POINT ( 'NONE', #13716 ) ;
#13039 = LINE ( 'NONE', #2449, #9452 ) ;
#13040 = CARTESIAN_POINT ( 'NONE',  ( -3.750000000000000000, 13.68750000000000178, -1.946699141100893149 ) ) ;
#13041 = DIRECTION ( 'NONE',  ( 0.000000000000000000, 1.000000000000000000, 0.000000000000000000 ) ) ;
#13042 = CARTESIAN_POINT ( 'NONE',  ( -63.42958736446724544, 11.57753352781592504, -203.1186045345161801 ) ) ;
#13043 = CARTESIAN_POINT ( 'NONE',  ( -4.545909498366142110, 5.000000000000000000, -129.6154209247606843 ) ) ;
#13044 = CARTESIAN_POINT ( 'NONE',  ( 3.249999999999998224, 4.187500000000000888, -4.846194077712561388 ) ) ;
#13045 = CARTESIAN_POINT ( 'NONE',  ( 6.288457687482224223, 8.673617379884035472E-16, -105.0111312234662506 ) ) ;
#13046 = PERSON_AND_ORGANIZATION ( #3176, #3020 ) ;
#13047 = CARTESIAN_POINT ( 'NONE',  ( -3.249999999999999556, 14.31250000000000000, -4.846194077712557835 ) ) ;
#13048 = CARTESIAN_POINT ( 'NONE',  ( -7.942089414655052693, 7.499999999999991118, -89.96019367200776173 ) ) ;
#13049 = VERTEX_POINT ( 'NONE', #12620 ) ;
#13050 = CARTESIAN_POINT ( 'NONE',  ( 7.113352963092393288, 0.9553916634466306235, 3.767908876148229780 ) ) ;
#13051 = CARTESIAN_POINT ( 'NONE',  ( -3.980102097228897245E-16, 1.500000000000000000, -6.749999999999999112 ) ) ;
#13052 = CARTESIAN_POINT ( 'NONE',  ( -8.562056237857618157, 0.7968074793529829059, -104.5167437574517919 ) ) ;
#13053 = CARTESIAN_POINT ( 'NONE',  ( -2.298097038856279362, 5.875000000000001776, -5.798097038856278473 ) ) ;
#13054 = ORIENTED_EDGE ( 'NONE', *, *, #4803, .F. ) ;
#13055 = CARTESIAN_POINT ( 'NONE',  ( -0.2812006908208667388, 15.00000000000000000, -110.9708452933458176 ) ) ;
#13056 =( BOUNDED_SURFACE ( )  B_SPLINE_SURFACE ( 3, 3, ( 
 ( #407, #7272, #9831, #2491, #329, #11986, #1409 ),
 ( #5196, #9910, #14406, #11908, #8509, #173, #245 ),
 ( #1333, #2571, #10991, #5042, #10827, #8585, #4880 ),
 ( #6036, #13244, #2647, #12062, #1480, #6195, #14488 ) ),
 .UNSPECIFIED., .F., .F., .F. ) 
 B_SPLINE_SURFACE_WITH_KNOTS ( ( 4, 4 ),
 ( 4, 3, 4 ),
 ( 0.000000000000000000, 1.000000000000000000 ),
 ( 0.000000000000000000, 0.5000000000000000000, 1.000000000000000000 ),
 .UNSPECIFIED. ) 
 GEOMETRIC_REPRESENTATION_ITEM ( )  RATIONAL_B_SPLINE_SURFACE ( (
 ( 1.000000000000000000, 0.7662986988867873661, 0.7662986988867873661, 1.000000000000000000, 0.7662986988867873661, 0.7662986988867873661, 1.000000000000000000),
 ( 0.9216682375510407699, 0.7062731712406410400, 0.7062731712406410400, 0.9216682375510407699, 0.7062731712406410400, 0.7062731712406410400, 0.9216682375510407699),
 ( 0.9216682375510407699, 0.7062731712406410400, 0.7062731712406410400, 0.9216682375510407699, 0.7062731712406410400, 0.7062731712406410400, 0.9216682375510407699),
 ( 1.000000000000000000, 0.7662986988867873661, 0.7662986988867873661, 1.000000000000000000, 0.7662986988867873661, 0.7662986988867873661, 1.000000000000000000) ) ) 
 REPRESENTATION_ITEM ( '' )  SURFACE ( )  );
#13057 = FACE_OUTER_BOUND ( 'NONE', #8990, .T. ) ;
#13058 = CARTESIAN_POINT ( 'NONE',  ( -3.249999999999999556, 2.312500000000000888, -4.846194077712557835 ) ) ;
#13059 = CARTESIAN_POINT ( 'NONE',  ( 1.553300858899109071, 2.437500000000000444, 0.2499999999999989175 ) ) ;
#13060 = CARTESIAN_POINT ( 'NONE',  ( -3.750000000000000000, 6.312500000000000000, -5.053300858899105741 ) ) ;
#13061 = FACE_BOUND ( 'NONE', #5791, .T. ) ;
#13062 = CARTESIAN_POINT ( 'NONE',  ( 3.749999999999999556, 7.250000000000001776, -3.500000000000000444 ) ) ;
#13063 = CARTESIAN_POINT ( 'NONE',  ( 4.739705316375511401, 14.53460293427037620, 1.305582433210761062 ) ) ;
#13064 = CARTESIAN_POINT ( 'NONE',  ( -3.802759337645547522, 10.36768682443087286, -43.20025118941907749 ) ) ;
#13065 = CARTESIAN_POINT ( 'NONE',  ( 17.21360758414088465, 4.000000000000000000, -156.8016104511478090 ) ) ;
#13066 = ADVANCED_FACE ( 'NONE', ( #4282 ), #15066, .T. ) ;
#13067 = CARTESIAN_POINT ( 'NONE',  ( 1.114947364559086829, 5.000000000000000888, -139.4079432275550232 ) ) ;
#13068 = CARTESIAN_POINT ( 'NONE',  ( 0.000000000000000000, 11.00000000000000000, -0.2500000000000002220 ) ) ;
#13069 = CARTESIAN_POINT ( 'NONE',  ( -4.090890948359609425, 15.00000000000000000, -103.1929727064838289 ) ) ;
#13070 = DIRECTION ( 'NONE',  ( -0.000000000000000000, -1.000000000000000000, -0.000000000000000000 ) ) ;
#13071 = ORIENTED_EDGE ( 'NONE', *, *, #5349, .T. ) ;
#13072 = LOCAL_TIME ( 12, 28, 20.00000000000000000, #12499 ) ;
#13073 = ORIENTED_EDGE ( 'NONE', *, *, #9105, .T. ) ;
#13074 = CARTESIAN_POINT ( 'NONE',  ( -6.279162093004023504, 4.336808689942017736E-16, -108.6370948588635912 ) ) ;
#13075 = CARTESIAN_POINT ( 'NONE',  ( -29.27234010639886108, 8.673617379884035472E-16, -207.3549529969440357 ) ) ;
#13076 = CARTESIAN_POINT ( 'NONE',  ( 0.000000000000000000, 4.000000000000000000, 0.2500000000000002220 ) ) ;
#13077 = CARTESIAN_POINT ( 'NONE',  ( -3.750000000000000000, 4.812500000000000000, -5.053300858899105741 ) ) ;
#13078 = AXIS2_PLACEMENT_3D ( 'NONE', #7596, #7676, #11236 ) ;
#13079 = CARTESIAN_POINT ( 'NONE',  ( -4.445322652854981627, 4.676033161754593892E-16, 1.000000000000000000 ) ) ;
#13080 = ORIENTED_EDGE ( 'NONE', *, *, #4223, .F. ) ;
#13081 = CARTESIAN_POINT ( 'NONE',  ( -5.561182064722144602, 0.1084047942993575236, -117.2542806587631787 ) ) ;
#13082 = CARTESIAN_POINT ( 'NONE',  ( 1.346194077712558279, 6.062500000000000000, -6.750000000000000888 ) ) ;
#13083 = CARTESIAN_POINT ( 'NONE',  ( -62.69788784789734137, 15.00000000000000000, -176.6065371158525181 ) ) ;
#13084 = LOCAL_TIME ( 12, 28, 20.00000000000000000, #894 ) ;
#13085 = DIRECTION ( 'NONE',  ( 0.000000000000000000, 0.000000000000000000, -1.000000000000000000 ) ) ;
#13086 = CARTESIAN_POINT ( 'NONE',  ( -3.249999999999999556, 8.312500000000000000, -4.846194077712557835 ) ) ;
#13087 = CIRCLE ( 'NONE', #2474, 2.999999999999999112 ) ;
#13088 = CONTEXT_DEPENDENT_SHAPE_REPRESENTATION ( #9858, #5954 ) ;
#13089 = B_SPLINE_CURVE_WITH_KNOTS ( 'NONE', 3,
 ( #14831, #12410, #4378, #9087, #4230, #13892, #2059, #6771, #10095, #970, #11408, #13736, #8935, #7849, #6541, #14982, #1906, #1832, #11254, #11328, #747, #5458, #10175, #1978, #6694, #826, #14268, #2286, #11929, #14193, #9385, #2431, #9313, #7125, #15136, #9542, #7209, #6991 ),
 .UNSPECIFIED., .F., .F.,
 ( 4, 2, 2, 2, 2, 2, 2, 2, 2, 2, 2, 2, 2, 2, 2, 2, 2, 2, 4 ),
 ( 0.000000000000000000, 0.005132352563142216634, 0.01026470512628443327, 0.02052941025256887000, 0.03079411537885330674, 0.03336029166042438210, 0.03592646794199545746, 0.04105882050513753184, 0.05132352563142168755, 0.05388970191299279067, 0.05645587819456389378, 0.06158823075770617633, 0.06672058332084844501, 0.07185293588399073450, 0.07441911216556192088, 0.07698528844713309338, 0.07955146472870427976, 0.08083455286948990071, 0.08211764101027552165 ),
 .UNSPECIFIED. ) ;
#13090 = ADVANCED_FACE ( 'NONE', ( #5651 ), #11868, .F. ) ;
#13091 = CARTESIAN_POINT ( 'NONE',  ( 8.610575960386558592, 15.00000000000000000, -106.0856774745618480 ) ) ;
#13092 = CARTESIAN_POINT ( 'NONE',  ( 25.37357285196682355, 5.000000000000000888, -136.0302139098317298 ) ) ;
#13093 = ORIENTED_EDGE ( 'NONE', *, *, #4492, .F. ) ;
#13094 = EDGE_CURVE ( 'NONE', #973, #9864, #4631, .T. ) ;
#13095 = CARTESIAN_POINT ( 'NONE',  ( -0.6328346815827367022, 15.00000000000000000, -109.3684695446412007 ) ) ;
#13096 = CYLINDRICAL_SURFACE ( 'NONE', #14100, 2.000000000000000000 ) ;
#13097 = ORIENTED_EDGE ( 'NONE', *, *, #7385, .F. ) ;
#13098 = EDGE_LOOP ( 'NONE', ( #1197, #5156, #6317, #10552 ) ) ;
#13099 = CARTESIAN_POINT ( 'NONE',  ( -0.3766621274091715987, 0.2004420829692335482, 0.1491815183709511161 ) ) ;
#13100 = CARTESIAN_POINT ( 'NONE',  ( -3.749999999999999556, 5.750000000000000888, -3.499999999999999112 ) ) ;
#13101 = CARTESIAN_POINT ( 'NONE',  ( 3.249999999999998224, 12.31250000000000178, -2.153805922287439945 ) ) ;
#13102 = ORIENTED_EDGE ( 'NONE', *, *, #6697, .T. ) ;
#13103 = VECTOR ( 'NONE', #14504, 1000.000000000000000 ) ;
#13104 = CARTESIAN_POINT ( 'NONE',  ( -19.94423925787080520, 9.999999999999998224, -150.2885610952392597 ) ) ;
#13105 = CARTESIAN_POINT ( 'NONE',  ( -3.980102097228897245E-16, 8.500000000000000000, -6.749999999999999112 ) ) ;
#13106 = AXIS2_PLACEMENT_3D ( 'NONE', #11835, #1114, #11618 ) ;
#13107 = AXIS2_PLACEMENT_3D ( 'NONE', #14693, #4094, #12344 ) ;
#13108 = APPROVAL ( #8597, 'UNKNOWN' ) ;
#13109 = CARTESIAN_POINT ( 'NONE',  ( -5.211827599098144859, 2.500000000000000888, -114.7762467949656582 ) ) ;
#13110 = CARTESIAN_POINT ( 'NONE',  ( -38.28777827158674540, 9.999999999999994671, -156.7712049258111620 ) ) ;
#13111 = APPROVAL_DATE_TIME ( #8383, #12728 ) ;
#13112 = VECTOR ( 'NONE', #3174, 1000.000000000000000 ) ;
#13113 = EDGE_CURVE ( 'NONE', #3224, #2133, #1133, .T. ) ;
#13114 = CYLINDRICAL_SURFACE ( 'NONE', #13201, 3.000000000000005329 ) ;
#13115 = ADVANCED_FACE ( 'NONE', ( #9138 ), #1997, .T. ) ;
#13116 = EDGE_CURVE ( 'NONE', #6908, #14015, #9635, .T. ) ;
#13117 = ORIENTED_EDGE ( 'NONE', *, *, #10836, .F. ) ;
#13118 = CARTESIAN_POINT ( 'NONE',  ( -2.298097038856278473, 9.125000000000000000, -1.201902961143720416 ) ) ;
#13119 = DIRECTION ( 'NONE',  ( -0.000000000000000000, 1.000000000000000000, -0.000000000000000000 ) ) ;
#13120 = AXIS2_PLACEMENT_3D ( 'NONE', #6321, #4010, #293 ) ;
#13121 = B_SPLINE_CURVE_WITH_KNOTS ( 'NONE', 3,
 ( #9096, #9254, #3144, #5470, #12420, #4464, #5391, #10189, #1990, #13817, #14843, #9176, #5690, #13979, #7707, #13906, #686, #11497, #8012, #912, #6852, #3304, #11263, #10106, #3219, #8946, #982, #12739, #14922, #10260, #6630, #2148, #4318, #9022, #15149, #10414 ),
 .UNSPECIFIED., .F., .F.,
 ( 4, 2, 2, 2, 2, 2, 2, 2, 2, 2, 2, 2, 2, 2, 2, 2, 2, 4 ),
 ( 1.734723475976807094E-18, 0.001204836556977712577, 0.002409673113955423419, 0.004819346227910881533, 0.006024182784888610157, 0.007229019341866339647, 0.008433855898844067403, 0.009638692455821797761, 0.01204836556977721164, 0.01445803868373262899, 0.01566287524071035414, 0.01686771179768807583, 0.01927738491164353307, 0.02409673113955440593, 0.02891607736746527879, 0.03132575048142070828, 0.03373542359537614471, 0.03855476982328707308 ),
 .UNSPECIFIED. ) ;
#13122 = CARTESIAN_POINT ( 'NONE',  ( -3.749999999999999556, 14.75000000000000000, -3.499999999999999112 ) ) ;
#13123 = CARTESIAN_POINT ( 'NONE',  ( 1.123784099566545791, 4.588323854676484181, -139.4224385785465188 ) ) ;
#13124 = CARTESIAN_POINT ( 'NONE',  ( -63.98308214666035809, 12.44470469654490330, -210.8813308483144908 ) ) ;
#13125 = DIRECTION ( 'NONE',  ( 1.000000000000000000, 0.000000000000000000, 0.000000000000000000 ) ) ;
#13126 = CARTESIAN_POINT ( 'NONE',  ( 1.346194077712561166, 1.437500000000000000, -0.2500000000000011102 ) ) ;
#13127 = CARTESIAN_POINT ( 'NONE',  ( 10.79182909825924419, 3.336188342113987293, -106.9908110512689063 ) ) ;
#13128 = PERSON_AND_ORGANIZATION_ROLE ( 'creator' ) ;
#13129 = CARTESIAN_POINT ( 'NONE',  ( -5.020274906786214686, 13.64026223784254022, -125.1229904268055293 ) ) ;
#13130 = DIRECTION ( 'NONE',  ( 0.000000000000000000, 0.000000000000000000, -1.000000000000000000 ) ) ;
#13131 = APPROVAL_PERSON_ORGANIZATION ( #2147, #10017, #15067 ) ;
#13132 = ORIENTED_EDGE ( 'NONE', *, *, #13576, .F. ) ;
#13133 = CARTESIAN_POINT ( 'NONE',  ( 7.528205663287619309, 1.351247849200009732, 4.229918499259564868 ) ) ;
#13134 = CARTESIAN_POINT ( 'NONE',  ( 3.249999999999999556, 6.750000000000000000, -3.500000000000000000 ) ) ;
#13135 = CARTESIAN_POINT ( 'NONE',  ( -9.262026962547025732, 2.111446349724324101, -105.1717885830827441 ) ) ;
#13136 = CARTESIAN_POINT ( 'NONE',  ( -3.249999999999999112, 0.6875000000000000000, -2.153805922287440833 ) ) ;
#13137 = APPROVAL ( #1148, 'UNSPECIFIED' ) ;
#13138 = CARTESIAN_POINT ( 'NONE',  ( -3.249999999999999112, 5.812500000000000888, -4.846194077712558723 ) ) ;
#13139 = ORIENTED_EDGE ( 'NONE', *, *, #12319, .F. ) ;
#13140 = CARTESIAN_POINT ( 'NONE',  ( -7.230047174082840478, 9.999999999999998224, -120.6008656444815585 ) ) ;
#13141 = CARTESIAN_POINT ( 'NONE',  ( 3.014182204252355390, 14.56766260765297361, 0.5812518486166803333 ) ) ;
#13142 = CARTESIAN_POINT ( 'NONE',  ( 10.38363273743979498, 14.45937571482893524, -106.4521696696246522 ) ) ;
#13143 = CARTESIAN_POINT ( 'NONE',  ( 3.249999999999998668, 0.6875000000000000000, -4.846194077712560500 ) ) ;
#13144 = CARTESIAN_POINT ( 'NONE',  ( 1.553300858899105963, 1.062500000000000444, -7.249999999999999112 ) ) ;
#13145 = CARTESIAN_POINT ( 'NONE',  ( -2.651650429449553314, 7.375000000000000888, -6.151650429449552426 ) ) ;
#13146 = CC_DESIGN_SECURITY_CLASSIFICATION ( #13898, ( #10666 ) ) ;
#13147 = CARTESIAN_POINT ( 'NONE',  ( -4.019421728525986559, 11.03613295220510615, -46.74835841341517551 ) ) ;
#13148 = CARTESIAN_POINT ( 'NONE',  ( 1.553300858899109516, 4.437500000000001776, 0.2499999999999993616 ) ) ;
#13149 = CARTESIAN_POINT ( 'NONE',  ( 1.439432938296930198, 13.23249829686945311, 4.644450407911167034 ) ) ;
#13150 = CARTESIAN_POINT ( 'NONE',  ( -3.881302238640954361, 11.25545205242913127, -45.78502156705464898 ) ) ;
#13151 = CIRCLE ( 'NONE', #6481, 2.500000000000000444 ) ;
#13152 = DIRECTION ( 'NONE',  ( -0.9997619372588931741, -0.000000000000000000, -0.02181900108494707821 ) ) ;
#13153 = CARTESIAN_POINT ( 'NONE',  ( 1.041519256436020280, 5.000000000000000888, -139.4527716894433240 ) ) ;
#13154 = CARTESIAN_POINT ( 'NONE',  ( -2.298097038856278473, 12.12500000000000000, -1.201902961143720416 ) ) ;
#13155 =( BOUNDED_SURFACE ( )  B_SPLINE_SURFACE ( 3, 1, ( 
 ( #4055, #1881 ),
 ( #4129, #11228 ),
 ( #7588, #12304 ),
 ( #5282, #8906 ) ),
 .UNSPECIFIED., .F., .F., .T. ) 
 B_SPLINE_SURFACE_WITH_KNOTS ( ( 4, 4 ),
 ( 2, 2 ),
 ( 0.000000000000000000, 1.000000000000000000 ),
 ( 0.000000000000000000, 1.000000000000000000 ),
 .UNSPECIFIED. ) 
 GEOMETRIC_REPRESENTATION_ITEM ( )  RATIONAL_B_SPLINE_SURFACE ( (
 ( 1.000000000000000000, 1.000000000000000000),
 ( 0.9748717492153319286, 0.9748717492153319286),
 ( 0.9748717492153319286, 0.9748717492153319286),
 ( 1.000000000000000000, 1.000000000000000000) ) ) 
 REPRESENTATION_ITEM ( '' )  SURFACE ( )  );
#13156 = CARTESIAN_POINT ( 'NONE',  ( -9.721966606378851239, 5.000000000000000888, -116.3614657639809309 ) ) ;
#13157 = CYLINDRICAL_SURFACE ( 'NONE', #6160, 5.000000000000000888 ) ;
#13158 = ORIENTED_EDGE ( 'NONE', *, *, #5630, .T. ) ;
#13159 = CARTESIAN_POINT ( 'NONE',  ( -3.750000000000000000, 8.687499999999998224, -1.946699141100893149 ) ) ;
#13160 = VERTEX_POINT ( 'NONE', #11384 ) ;
#13161 = CARTESIAN_POINT ( 'NONE',  ( -5.462587733787561461, 4.336808689942017736E-16, -110.6302725851879529 ) ) ;
#13162 = CARTESIAN_POINT ( 'NONE',  ( -23.51189632655365003, -2.261592833039957532E-12, -204.5548166363960547 ) ) ;
#13163 = CARTESIAN_POINT ( 'NONE',  ( -3.750000000000000000, 8.250000000000000000, -3.499999999999999112 ) ) ;
#13164 = CARTESIAN_POINT ( 'NONE',  ( -3.749999999999999556, 3.750000000000000444, -3.499999999999999112 ) ) ;
#13165 = CARTESIAN_POINT ( 'NONE',  ( -9.030574454602197321, 2.490287375297123962, -34.97919997656152447 ) ) ;
#13166 = ORIENTED_EDGE ( 'NONE', *, *, #4195, .F. ) ;
#13167 = TOROIDAL_SURFACE ( 'NONE', #6251, 4.000000000000001776, 1.000000000000000000 ) ;
#13168 = CARTESIAN_POINT ( 'NONE',  ( 2.298097038856279362, 3.375000000000000444, -1.201902961143720860 ) ) ;
#13169 = CARTESIAN_POINT ( 'NONE',  ( -70.10710660206702016, 15.00000000000000000, -192.1972859456651861 ) ) ;
#13170 = CARTESIAN_POINT ( 'NONE',  ( 11.73205471245423048, 8.673617379884034486E-16, -131.2319155360884793 ) ) ;
#13171 =( NAMED_UNIT ( * ) PLANE_ANGLE_UNIT ( ) SI_UNIT ( $, .RADIAN. ) );
#13172 = CARTESIAN_POINT ( 'NONE',  ( -3.980102097228897245E-16, 6.500000000000000888, -6.749999999999999112 ) ) ;
#13173 = CARTESIAN_POINT ( 'NONE',  ( -25.66911763371813038, -5.000000000000000888, -138.9799121221676046 ) ) ;
#13174 = SECURITY_CLASSIFICATION_LEVEL ( 'unclassified' ) ;
#13175 = CARTESIAN_POINT ( 'NONE',  ( -1.511057375649833556, 6.071532165918824830E-15, -124.5116290068135640 ) ) ;
#13176 = CARTESIAN_POINT ( 'NONE',  ( 18.82489474308959032, 5.000000000000000888, -131.0518286717021397 ) ) ;
#13177 = EDGE_LOOP ( 'NONE', ( #11932, #1889, #6326, #637 ) ) ;
#13178 = VECTOR ( 'NONE', #13850, 1000.000000000000000 ) ;
#13179 = CARTESIAN_POINT ( 'NONE',  ( -8.205916711996726676, 7.499999999999991118, -92.94857034792688921 ) ) ;
#13180 = VECTOR ( 'NONE', #2333, 1000.000000000000000 ) ;
#13181 = CARTESIAN_POINT ( 'NONE',  ( -3.249999999999999556, 14.25000000000000000, -3.499999999999999556 ) ) ;
#13182 = ORIENTED_EDGE ( 'NONE', *, *, #9427, .T. ) ;
#13183 = ORIENTED_EDGE ( 'NONE', *, *, #5262, .T. ) ;
#13184 = CARTESIAN_POINT ( 'NONE',  ( 26.26584183167803133, 2.580188100158157916, -138.3181169695228334 ) ) ;
#13185 = CARTESIAN_POINT ( 'NONE',  ( 0.000000000000000000, 13.50000000000000355, 0.2499999999999998057 ) ) ;
#13186 = CARTESIAN_POINT ( 'NONE',  ( -3.249999999999999112, 8.687499999999998224, -2.153805922287440833 ) ) ;
#13187 = ORIENTED_EDGE ( 'NONE', *, *, #4618, .T. ) ;
#13188 = CARTESIAN_POINT ( 'NONE',  ( -4.781971238311125916, 15.00000000000000000, -110.8602639898872155 ) ) ;
#13189 = CARTESIAN_POINT ( 'NONE',  ( 2.298097038856279362, 7.875000000000000000, -1.201902961143720860 ) ) ;
#13190 = B_SPLINE_CURVE_WITH_KNOTS ( 'NONE', 3,
 ( #4136, #8913, #3904, #2895, #425, #3043, #7754, #12469, #498, #1888 ),
 .UNSPECIFIED., .F., .F.,
 ( 4, 2, 2, 2, 4 ),
 ( 0.000000000000000000, 0.0005552365111544495723, 0.001110473022308899145, 0.001665709533463348609, 0.002220946044617798289 ),
 .UNSPECIFIED. ) ;
#13191 = ADVANCED_FACE ( 'NONE', ( #655 ), #8224, .T. ) ;
#13192 = AXIS2_PLACEMENT_3D ( 'NONE', #5495, #1941, #11068 ) ;
#13193 = CIRCLE ( 'NONE', #9732, 5.000000000000004441 ) ;
#13194 = CARTESIAN_POINT ( 'NONE',  ( -7.490046183253692647, 0.1222994804349853415, -104.2926538792397508 ) ) ;
#13195 = CARTESIAN_POINT ( 'NONE',  ( -52.88346389043234552, 9.999999999999996447, -169.0946036997559929 ) ) ;
#13196 = CARTESIAN_POINT ( 'NONE',  ( -76.20282042307043469, 5.000000000000000888, -188.4633497277649496 ) ) ;
#13197 = DATE_TIME_ROLE ( 'classification_date' ) ;
#13198 = CARTESIAN_POINT ( 'NONE',  ( 11.74818764249840797, 15.00000000000000000, -127.4816575577899584 ) ) ;
#13199 = ORIENTED_EDGE ( 'NONE', *, *, #10642, .F. ) ;
#13200 = CARTESIAN_POINT ( 'NONE',  ( 3.249999999999999556, 1.750000000000000000, -3.500000000000000000 ) ) ;
#13201 = AXIS2_PLACEMENT_3D ( 'NONE', #2527, #14204, #4763 ) ;
#13202 = LINE ( 'NONE', #1369, #3779 ) ;
#13203 = EDGE_CURVE ( 'NONE', #3391, #15055, #8120, .T. ) ;
#13204 = CARTESIAN_POINT ( 'NONE',  ( 1.553300858899105963, 15.06250000000000178, -7.249999999999999112 ) ) ;
#13205 = ADVANCED_FACE ( 'NONE', ( #11902 ), #5872, .T. ) ;
#13206 = ADVANCED_FACE ( 'NONE', ( #12849 ), #5454, .T. ) ;
#13207 = CARTESIAN_POINT ( 'NONE',  ( -63.55690675229147502, 11.98211585306279581, -202.8120525166195875 ) ) ;
#13208 = CARTESIAN_POINT ( 'NONE',  ( -0.2500000000000000555, 5.000000000000000000, 1.500000000000000222 ) ) ;
#13209 = CARTESIAN_POINT ( 'NONE',  ( -2.298097038856278029, 1.625000000000000000, -1.201902961143720638 ) ) ;
#13210 = CARTESIAN_POINT ( 'NONE',  ( 10.23916242951791844, 1.886766667146307919, -106.0869873573526263 ) ) ;
#13211 = APPROVAL_DATE_TIME ( #1682, #10068 ) ;
#13212 = CIRCLE ( 'NONE', #9755, 1.250000000000005107 ) ;
#13213 = CARTESIAN_POINT ( 'NONE',  ( -3.674418796289115718, 14.44898052987122128, -125.2714716606675722 ) ) ;
#13214 = CARTESIAN_POINT ( 'NONE',  ( -16.72147566907574756, 0.2067131101362160162, -130.8524528097921404 ) ) ;
#13215 = VERTEX_POINT ( 'NONE', #2485 ) ;
#13216 = CARTESIAN_POINT ( 'NONE',  ( 7.530864077104208576, 1.500743522379207606, 1.949903166259959297 ) ) ;
#13217 = CARTESIAN_POINT ( 'NONE',  ( -3.249999999999999556, 8.250000000000000000, -3.499999999999999556 ) ) ;
#13218 = CARTESIAN_POINT ( 'NONE',  ( -8.943845545880508396, 1.244574210897673616, -105.0375473151879362 ) ) ;
#13219 = CARTESIAN_POINT ( 'NONE',  ( 2.298097038856278473, 13.62500000000000000, -5.798097038856279362 ) ) ;
#13220 = CARTESIAN_POINT ( 'NONE',  ( 3.249999999999999556, 8.250000000000000000, -3.500000000000000000 ) ) ;
#13221 = CARTESIAN_POINT ( 'NONE',  ( -0.2151733755447025886, 15.00000000000000000, -115.1395769290326427 ) ) ;
#13222 = CARTESIAN_POINT ( 'NONE',  ( 0.000000000000000000, -0.2105996885190176415, -0.1347136637304948981 ) ) ;
#13223 = CARTESIAN_POINT ( 'NONE',  ( 9.412918133875843196, 14.94619758066195914, -106.0880953390660579 ) ) ;
#13224 = CARTESIAN_POINT ( 'NONE',  ( -2.298097038856278473, 2.125000000000000000, -1.201902961143720416 ) ) ;
#13225 = CARTESIAN_POINT ( 'NONE',  ( -1.553300858899107073, 2.937500000000000444, -7.249999999999999112 ) ) ;
#13226 = ADVANCED_FACE ( 'NONE', ( #5804 ), #8343, .T. ) ;
#13227 =( REPRESENTATION_RELATIONSHIP ('NONE','NONE', #11394, #12477 ) REPRESENTATION_RELATIONSHIP_WITH_TRANSFORMATION ( #7200 )SHAPE_REPRESENTATION_RELATIONSHIP( ) );
#13228 = CARTESIAN_POINT ( 'NONE',  ( -3.750000000000000000, 5.312500000000000888, -5.053300858899105741 ) ) ;
#13229 = CC_DESIGN_PERSON_AND_ORGANIZATION_ASSIGNMENT ( #3373, #4615, ( #5834 ) ) ;
#13230 = CARTESIAN_POINT ( 'NONE',  ( 0.2177290144686464812, 3.455212393055724807, 2.466220573332666088 ) ) ;
#13231 = CARTESIAN_POINT ( 'NONE',  ( -3.750000000000000000, 4.812500000000001776, -5.053300858899105741 ) ) ;
#13232 = CARTESIAN_POINT ( 'NONE',  ( 0.5471942990909076654, 10.82315019902009290, 5.691692885981924022 ) ) ;
#13233 = CARTESIAN_POINT ( 'NONE',  ( 12.37900876701962360, 2.133003846422337535, -165.9182586569806404 ) ) ;
#13234 = CARTESIAN_POINT ( 'NONE',  ( -6.683304552674626642, 0.000000000000000000, -104.1296019027811894 ) ) ;
#13235 = CARTESIAN_POINT ( 'NONE',  ( 3.249999999999999112, 10.81250000000000178, -2.153805922287439945 ) ) ;
#13236 = CARTESIAN_POINT ( 'NONE',  ( -9.335177092165887203, 3.999999999999993783, -147.7150205453479543 ) ) ;
#13237 = CARTESIAN_POINT ( 'NONE',  ( 3.249999999999998668, 14.68750000000000000, -4.846194077712560500 ) ) ;
#13238 = CARTESIAN_POINT ( 'NONE',  ( -22.81000397151760239, 8.673617379884034486E-16, -177.4076321631416704 ) ) ;
#13239 = CARTESIAN_POINT ( 'NONE',  ( -63.21422130130007133, 9.999999999999998224, -203.6040552426024703 ) ) ;
#13240 = VERTEX_POINT ( 'NONE', #91 ) ;
#13241 = CARTESIAN_POINT ( 'NONE',  ( 2.651650429449552870, 11.12500000000000000, -6.151650429449555091 ) ) ;
#13242 = VERTEX_POINT ( 'NONE', #2262 ) ;
#13243 = CARTESIAN_POINT ( 'NONE',  ( -5.145745206718213893, 2.650598460978550256E-13, -112.5500021907200363 ) ) ;
#13244 = CARTESIAN_POINT ( 'NONE',  ( 9.458437899194636955, 0.000000000000000000, -40.77697206847473410 ) ) ;
#13245 = CARTESIAN_POINT ( 'NONE',  ( 3.750000000000000000, 10.75000000000000000, -3.500000000000000444 ) ) ;
#13246 = CARTESIAN_POINT ( 'NONE',  ( 0.000000000000000000, 6.500000000000000000, 0.2499999999999998057 ) ) ;
#13247 = LINE ( 'NONE', #1254, #4046 ) ;
#13248 = ORIENTED_EDGE ( 'NONE', *, *, #14514, .T. ) ;
#13249 = CARTESIAN_POINT ( 'NONE',  ( -3.249999999999999556, 5.750000000000000000, -3.500000000000000000 ) ) ;
#13250 = EDGE_CURVE ( 'NONE', #8996, #13395, #10526, .T. ) ;
#13251 = CARTESIAN_POINT ( 'NONE',  ( -1.553300858899106629, 10.06250000000000000, 0.2500000000000002220 ) ) ;
#13252 = CARTESIAN_POINT ( 'NONE',  ( -69.57949925813656478, 15.00000000000227907, -184.9351518006187121 ) ) ;
#13253 = PLANE ( 'NONE',  #13833 ) ;
#13254 = CARTESIAN_POINT ( 'NONE',  ( 1.346194077712558057, 8.562500000000001776, -6.750000000000000000 ) ) ;
#13255 = CALENDAR_DATE ( 2026, 8, 10 ) ;
#13256 = CARTESIAN_POINT ( 'NONE',  ( -1.445049719264795529, 1.188659952750201131E-12, -134.5128495246223110 ) ) ;
#13257 = CARTESIAN_POINT ( 'NONE',  ( 8.769209038339429441, 5.000000000000000888, -110.8932515380079025 ) ) ;
#13258 = VERTEX_POINT ( 'NONE', #9359 ) ;
#13259 = DIRECTION ( 'NONE',  ( -1.000000000000000000, 0.000000000000000000, -0.000000000000000000 ) ) ;
#13260 = FACE_OUTER_BOUND ( 'NONE', #1686, .T. ) ;
#13261 = ORIENTED_EDGE ( 'NONE', *, *, #13113, .T. ) ;
#13262 = ORIENTED_EDGE ( 'NONE', *, *, #10014, .F. ) ;
#13263 = CARTESIAN_POINT ( 'NONE',  ( 26.36813061592906138, 2.735303735283647786, -138.3050569091936097 ) ) ;
#13264 = CARTESIAN_POINT ( 'NONE',  ( -3.750000000000000000, 11.81250000000000178, -5.053300858899105741 ) ) ;
#13265 = CARTESIAN_POINT ( 'NONE',  ( 1.346194077712558279, 7.062499999999999112, -6.750000000000000888 ) ) ;
#13266 = CARTESIAN_POINT ( 'NONE',  ( 1.346194077712558279, 9.062500000000000000, -6.750000000000000888 ) ) ;
#13267 = EDGE_LOOP ( 'NONE', ( #14587, #405, #2385, #2037 ) ) ;
#13268 = CARTESIAN_POINT ( 'NONE',  ( 5.000000000000001776, 15.00000000000000000, -1.663700395152567513 ) ) ;
#13269 = CARTESIAN_POINT ( 'NONE',  ( -1.346194077712559389, 7.437500000000000888, -6.749999999999999112 ) ) ;
#13270 = VECTOR ( 'NONE', #8500, 1000.000000000000000 ) ;
#13271 = CARTESIAN_POINT ( 'NONE',  ( -8.887479029472178382, 1.222969012369685915, -104.5864904545480556 ) ) ;
#13272 = CARTESIAN_POINT ( 'NONE',  ( -60.26128208755820026, 10.00000000000000178, -186.2863115604802431 ) ) ;
#13273 = CARTESIAN_POINT ( 'NONE',  ( 4.554677347145018373, -2.225540348348185052E-17, -1.000000000000000000 ) ) ;
#13274 = APPROVAL_STATUS ( 'not_yet_approved' ) ;
#13275 = CARTESIAN_POINT ( 'NONE',  ( -25.33202823091587774, 0.2517120273413803733, -202.7304169256179307 ) ) ;
#13276 = EDGE_CURVE ( 'NONE', #5602, #11406, #12939, .T. ) ;
#13277 = AXIS2_PLACEMENT_3D ( 'NONE', #10840, #8909, #12539 ) ;
#13278 = ORIENTED_EDGE ( 'NONE', *, *, #7883, .T. ) ;
#13279 = EDGE_CURVE ( 'NONE', #6539, #114, #14786, .T. ) ;
#13280 = CARTESIAN_POINT ( 'NONE',  ( 1.346194077712561166, 14.43750000000000178, -0.2500000000000011102 ) ) ;
#13281 = CARTESIAN_POINT ( 'NONE',  ( -3.749999999999999556, 13.31250000000000000, -5.053300858899104853 ) ) ;
#13282 = DIRECTION ( 'NONE',  ( 0.000000000000000000, -1.000000000000000000, 0.000000000000000000 ) ) ;
#13283 = CARTESIAN_POINT ( 'NONE',  ( 3.749999999999998668, 13.18750000000000000, -5.053300858899108405 ) ) ;
#13284 = CARTESIAN_POINT ( 'NONE',  ( -65.68091296275530055, 15.20918062550879313, -202.8221454773010635 ) ) ;
#13285 = CARTESIAN_POINT ( 'NONE',  ( -13.50872241962065701, 7.499999999999991118, -90.47263585218773585 ) ) ;
#13286 = CARTESIAN_POINT ( 'NONE',  ( -1.346194077712558945, 2.562500000000000444, -0.2500000000000002220 ) ) ;
#13287 = CARTESIAN_POINT ( 'NONE',  ( 10.45437233589498760, 14.39522854901148996, -106.2185126042158743 ) ) ;
#13288 = APPROVAL_DATE_TIME ( #11953, #10863 ) ;
#13289 = CARTESIAN_POINT ( 'NONE',  ( -65.69798262610476058, 14.93413372664151595, -187.7077297338020969 ) ) ;
#13290 = LINE ( 'NONE', #299, #9395 ) ;
#13291 = ORIENTED_EDGE ( 'NONE', *, *, #4932, .T. ) ;
#13292 = CARTESIAN_POINT ( 'NONE',  ( 4.625401223603891943, 0.004023134192272380567, -0.5198385758609599394 ) ) ;
#13293 = CARTESIAN_POINT ( 'NONE',  ( -3.249999999999999556, 6.187500000000000000, -2.153805922287440833 ) ) ;
#13294 = EDGE_CURVE ( 'NONE', #973, #12551, #8658, .T. ) ;
#13295 = CARTESIAN_POINT ( 'NONE',  ( -67.73240446793354863, 10.00000000000000000, -176.0047139660857169 ) ) ;
#13296 = CARTESIAN_POINT ( 'NONE',  ( 0.000000000000000000, 13.00000000000000178, -0.2500000000000002220 ) ) ;
#13297 = CARTESIAN_POINT ( 'NONE',  ( 0.000000000000000000, 10.49999999999999822, -0.2500000000000002220 ) ) ;
#13298 = CARTESIAN_POINT ( 'NONE',  ( -3.366457130219030702, 15.00000000000000000, -104.0285275769127651 ) ) ;
#13299 = DIRECTION ( 'NONE',  ( -0.000000000000000000, -1.000000000000000000, -0.000000000000000000 ) ) ;
#13300 = FACE_OUTER_BOUND ( 'NONE', #10495, .T. ) ;
#13301 = CARTESIAN_POINT ( 'NONE',  ( -1.346194077712559389, 5.062500000000001776, -0.2500000000000002220 ) ) ;
#13302 = CARTESIAN_POINT ( 'NONE',  ( 1.346194077712558279, 15.06250000000000178, -6.750000000000000888 ) ) ;
#13303 = B_SPLINE_CURVE_WITH_KNOTS ( 'NONE', 3,
 ( #7892, #9208, #15256, #5578, #2030, #2258, #8044, #5801, #12924, #4726, #4647, #8117, #8194, #9356, #6963, #12693, #12844, #2179, #14082, #6883 ),
 .UNSPECIFIED., .F., .F.,
 ( 4, 2, 2, 2, 2, 2, 2, 2, 2, 4 ),
 ( -1.419801435424954991E-05, 0.001093604629081186205, 0.002201407272516621959, 0.003309209915952058146, 0.004417012559387493466, 0.005524815202822929219, 0.006078716524540635387, 0.006632617846258340687, 0.007740420489693738276, 0.008848223133129131529 ),
 .UNSPECIFIED. ) ;
#13304 = CARTESIAN_POINT ( 'NONE',  ( 3.749999999999999556, 6.812500000000000000, -1.946699141100892261 ) ) ;
#13305 = CARTESIAN_POINT ( 'NONE',  ( -4.002681499858608660, 10.63006427533628440, -45.31489617893276289 ) ) ;
#13306 = CARTESIAN_POINT ( 'NONE',  ( 3.749999999999999556, 5.250000000000000000, -3.500000000000000444 ) ) ;
#13307 = CARTESIAN_POINT ( 'NONE',  ( 1.208030854046586722, 12.86766912361566817, 4.923196339896195539 ) ) ;
#13308 = CARTESIAN_POINT ( 'NONE',  ( 11.04730217088350663, 12.49999999999999822, -107.1178495010082941 ) ) ;
#13309 = DIRECTION ( 'NONE',  ( 0.000000000000000000, 0.000000000000000000, 1.000000000000000000 ) ) ;
#13310 = CARTESIAN_POINT ( 'NONE',  ( 1.592538968424295431, 8.673617379884034486E-16, -140.1913613025302254 ) ) ;
#13311 = DIRECTION ( 'NONE',  ( 0.000000000000000000, 1.000000000000000000, 0.000000000000000000 ) ) ;
#13312 = ADVANCED_FACE ( 'NONE', ( #5192 ), #14558, .F. ) ;
#13313 = CARTESIAN_POINT ( 'NONE',  ( -10.59012558253652792, 8.673617379884035472E-16, -156.2763189018182857 ) ) ;
#13314 = ORIENTED_EDGE ( 'NONE', *, *, #12014, .T. ) ;
#13315 = CARTESIAN_POINT ( 'NONE',  ( 2.651650429449554203, 13.37500000000000000, -0.8483495705504471296 ) ) ;
#13316 = ORIENTED_EDGE ( 'NONE', *, *, #2523, .T. ) ;
#13317 = CARTESIAN_POINT ( 'NONE',  ( -6.654685604018685474, 2.500000000000000444, -108.0058818678391077 ) ) ;
#13318 = CARTESIAN_POINT ( 'NONE',  ( -24.74264876967802351, 4.000000000000000888, -209.2209370252883787 ) ) ;
#13319 = CARTESIAN_POINT ( 'NONE',  ( 2.651650429449553759, 10.87500000000000178, -0.8483495705504471296 ) ) ;
#13320 = CARTESIAN_POINT ( 'NONE',  ( -3.749999999999999556, 7.750000000000000888, -3.499999999999999112 ) ) ;
#13321 = DIRECTION ( 'NONE',  ( 0.000000000000000000, 0.000000000000000000, 1.000000000000000000 ) ) ;
#13322 = ORIENTED_EDGE ( 'NONE', *, *, #2215, .T. ) ;
#13323 = PERSON ( 'NAUO-PER3', 'UNSPECIFIED', 'UNSPECIFIED', ('UNSPECIFIED'), ('UNSPECIFIED'), ('UNSPECIFIED') ) ;
#13324 = CARTESIAN_POINT ( 'NONE',  ( -1.346194077712559167, 5.937500000000000000, -6.749999999999999112 ) ) ;
#13325 = B_SPLINE_CURVE_WITH_KNOTS ( 'NONE', 3,
 ( #5646, #10364, #10143, #2028, #4498, #9131, #13711, #8043, #4575, #5424 ),
 .UNSPECIFIED., .F., .F.,
 ( 4, 2, 2, 2, 4 ),
 ( 0.000000000000000000, 0.0009395823385051277950, 0.001879164677010255590, 0.002818747015515383168, 0.003758329354020511180 ),
 .UNSPECIFIED. ) ;
#13326 = B_SPLINE_CURVE_WITH_KNOTS ( 'NONE', 3,
 ( #1300, #13129, #10726, #7240, #11954, #13213, #1379, #6081, #212, #4926, #3774, #8479 ),
 .UNSPECIFIED., .F., .F.,
 ( 4, 2, 2, 2, 2, 4 ),
 ( 0.000000000000000000, 0.001181812431113227766, 0.001772718646669842841, 0.002363624862226459001, 0.003545437293339693055, 0.004727249724452926675 ),
 .UNSPECIFIED. ) ;
#13327 = CARTESIAN_POINT ( 'NONE',  ( -2.651650429449552870, 10.12500000000000000, -0.8483495705504462414 ) ) ;
#13328 = CARTESIAN_POINT ( 'NONE',  ( -66.67437826168175263, 9.999999999999998224, -172.5466827975655235 ) ) ;
#13329 = CARTESIAN_POINT ( 'NONE',  ( 7.148068729939693000, 2.490287375297123518, -34.56909192082981974 ) ) ;
#13330 = CARTESIAN_POINT ( 'NONE',  ( -3.980102097228897245E-16, 9.500000000000000000, -6.749999999999999112 ) ) ;
#13331 = CARTESIAN_POINT ( 'NONE',  ( -5.418138540701908923, 15.00000000000000711, -127.8817495432483469 ) ) ;
#13332 = DATE_AND_TIME ( #6289, #8893 ) ;
#13333 = CARTESIAN_POINT ( 'NONE',  ( -2.629469332551699789, -8.673617379884035472E-16, -121.9913505756445886 ) ) ;
#13334 = FACE_OUTER_BOUND ( 'NONE', #15197, .T. ) ;
#13335 = ORIENTED_EDGE ( 'NONE', *, *, #11420, .F. ) ;
#13336 = CARTESIAN_POINT ( 'NONE',  ( 30.32986759126112730, 1.750000000000000000, 46.54214087805580391 ) ) ;
#13337 = DIRECTION ( 'NONE',  ( 0.000000000000000000, 0.000000000000000000, -1.000000000000000000 ) ) ;
#13338 = EDGE_LOOP ( 'NONE', ( #14263, #13025, #9066, #4672, #11629, #14770 ) ) ;
#13339 = ORIENTED_EDGE ( 'NONE', *, *, #7139, .F. ) ;
#13340 = CARTESIAN_POINT ( 'NONE',  ( 22.68437819464854854, 0.2142782701973315329, -138.7614552119420352 ) ) ;
#13341 = CARTESIAN_POINT ( 'NONE',  ( 3.749999999999999556, 13.25000000000000178, -3.500000000000000444 ) ) ;
#13342 = CARTESIAN_POINT ( 'NONE',  ( -3.980102097228897738E-16, 13.00000000000000000, -6.749999999999999112 ) ) ;
#13343 = CARTESIAN_POINT ( 'NONE',  ( 1.346194077712558279, 11.06250000000000178, -6.750000000000000888 ) ) ;
#13344 = ORIENTED_EDGE ( 'NONE', *, *, #13557, .F. ) ;
#13345 = DIRECTION ( 'NONE',  ( 8.764770998266003672E-18, -0.000000000000000000, 1.000000000000000000 ) ) ;
#13346 = CARTESIAN_POINT ( 'NONE',  ( -3.249999999999999556, 8.187500000000000000, -2.153805922287440833 ) ) ;
#13347 = CC_DESIGN_APPROVAL ( #12267, ( #12090 ) ) ;
#13348 = AXIS2_PLACEMENT_3D ( 'NONE', #11606, #4428, #14964 ) ;
#13349 = FACE_BOUND ( 'NONE', #14582, .T. ) ;
#13350 = CARTESIAN_POINT ( 'NONE',  ( -57.00133116092639796, 10.00000000000000000, -176.8568458259982776 ) ) ;
#13351 = CALENDAR_DATE ( 2026, 8, 10 ) ;
#13352 = DIRECTION ( 'NONE',  ( 0.9961255586397055328, 0.000000000000000000, -0.08794243244722427244 ) ) ;
#13353 = ORGANIZATION ( 'NAUO-ORG4', 'UNSPECIFIED', 'UNSPECIFIED' ) ;
#13354 = EDGE_LOOP ( 'NONE', ( #13010, #3833, #8542, #11080, #14436, #22, #6473, #5755, #3573, #4750, #10153, #8221, #9792 ) ) ;
#13355 = CARTESIAN_POINT ( 'NONE',  ( -3.980102097228897245E-16, 9.500000000000000000, -6.749999999999999112 ) ) ;
#13356 = CARTESIAN_POINT ( 'NONE',  ( 0.000000000000000000, 0.000000000000000000, -0.2500000000000002220 ) ) ;
#13357 = CARTESIAN_POINT ( 'NONE',  ( 3.750000000000000000, 11.75000000000000000, -3.500000000000000444 ) ) ;
#13358 = AXIS2_PLACEMENT_3D ( 'NONE', #11073, #2957, #14730 ) ;
#13359 = VECTOR ( 'NONE', #1763, 1000.000000000000000 ) ;
#13360 = CARTESIAN_POINT ( 'NONE',  ( -4.834347064118100334, 1.750000000000027756, 4.227958732727228330 ) ) ;
#13361 = EDGE_CURVE ( 'NONE', #5152, #933, #5904, .T. ) ;
#13362 = CARTESIAN_POINT ( 'NONE',  ( 1.553300858899108849, 1.937500000000000000, 0.2499999999999993616 ) ) ;
#13363 = AXIS2_PLACEMENT_3D ( 'NONE', #8685, #13420, #6366 ) ;
#13364 = CARTESIAN_POINT ( 'NONE',  ( -63.26674631656910464, 10.78987469582507508, -203.4893414402424412 ) ) ;
#13365 = CARTESIAN_POINT ( 'NONE',  ( -17.32624372123753886, 5.000000000000000000, -122.3796757791585321 ) ) ;
#13366 = CARTESIAN_POINT ( 'NONE',  ( 1.553300858899108849, 0.9375000000000000000, 0.2499999999999993616 ) ) ;
#13367 = AXIS2_PLACEMENT_3D ( 'NONE', #11021, #5146, #9857 ) ;
#13368 = CALENDAR_DATE ( 2026, 8, 10 ) ;
#13369 = DIRECTION ( 'NONE',  ( 0.000000000000000000, 0.000000000000000000, 1.000000000000000000 ) ) ;
#13370 = CARTESIAN_POINT ( 'NONE',  ( 7.000000000000000888, 9.999999999999998224, -1.663700395152567513 ) ) ;
#13371 = VERTEX_POINT ( 'NONE', #13394 ) ;
#13372 = CARTESIAN_POINT ( 'NONE',  ( 4.029045719581688445, 0.1039572972702087761, -1.052128926548778542 ) ) ;
#13373 = CARTESIAN_POINT ( 'NONE',  ( 3.249999999999999112, 6.812500000000000000, -2.153805922287439945 ) ) ;
#13374 = CARTESIAN_POINT ( 'NONE',  ( -9.285933597860747568, 2.305077891771167398, -105.1819416472893494 ) ) ;
#13375 = CARTESIAN_POINT ( 'NONE',  ( 2.298097038856279362, 14.87500000000000178, -1.201902961143720860 ) ) ;
#13376 = CIRCLE ( 'NONE', #9161, 0.5000000000000004441 ) ;
#13377 = CARTESIAN_POINT ( 'NONE',  ( -3.249999999999999112, 10.68750000000000178, -2.153805922287440833 ) ) ;
#13378 = CARTESIAN_POINT ( 'NONE',  ( 0.000000000000000000, 9.999999999999998224, -100.6237003951525679 ) ) ;
#13379 = CARTESIAN_POINT ( 'NONE',  ( 7.000000000000000888, 5.000000000000000888, -1.663700395152567513 ) ) ;
#13380 = CARTESIAN_POINT ( 'NONE',  ( 1.165583190371173750, 4.454698458770116609, -139.4098078394992228 ) ) ;
#13381 = CARTESIAN_POINT ( 'NONE',  ( -3.980102097228897245E-16, 3.500000000000000000, -6.749999999999999112 ) ) ;
#13382 = CARTESIAN_POINT ( 'NONE',  ( -2.651650429449552870, 3.875000000000000444, -6.151650429449552426 ) ) ;
#13383 = CARTESIAN_POINT ( 'NONE',  ( 1.553300858899105963, 10.56250000000000000, -7.250000000000000000 ) ) ;
#13384 = EDGE_CURVE ( 'NONE', #1192, #5201, #12294, .T. ) ;
#13385 = CARTESIAN_POINT ( 'NONE',  ( -3.345600617387282760, 10.60900084060682147, -45.14673711435018078 ) ) ;
#13386 = CARTESIAN_POINT ( 'NONE',  ( 1.553300858899105963, 5.062500000000000000, -7.250000000000000888 ) ) ;
#13387 = CARTESIAN_POINT ( 'NONE',  ( 3.292862661403878732, 11.00682189581027615, 5.097845610625860502 ) ) ;
#13388 = AXIS2_PLACEMENT_3D ( 'NONE', #8083, #12807, #6921 ) ;
#13389 = CARTESIAN_POINT ( 'NONE',  ( 6.369258321017760238, -2.529993217055220178, -34.56909192082981974 ) ) ;
#13390 =( BOUNDED_CURVE ( )  B_SPLINE_CURVE ( 3, ( #4861, #14227, #77, #2626 ),
 .UNSPECIFIED., .F., .T. ) 
 B_SPLINE_CURVE_WITH_KNOTS ( ( 4, 4 ),
 ( 3.820990438000858802, 4.241828308846971041 ),
 .UNSPECIFIED. ) 
 CURVE ( )  GEOMETRIC_REPRESENTATION_ITEM ( )  RATIONAL_B_SPLINE_CURVE ( ( 1.000000000000000000, 0.9852956651098603302, 0.9852956651098603302, 1.000000000000000000 ) ) 
 REPRESENTATION_ITEM ( '' )  );
#13391 = CARTESIAN_POINT ( 'NONE',  ( -17.32624372123753886, 9.999999999999998224, -134.3796757791585037 ) ) ;
#13392 = CARTESIAN_POINT ( 'NONE',  ( -4.808605925792019065, 8.673617379884035472E-16, -150.1721608607652456 ) ) ;
#13393 = PLANE ( 'NONE',  #9639 ) ;
#13394 = CARTESIAN_POINT ( 'NONE',  ( 7.347880794884122694E-16, 1.000000000000000000, 6.000000000000002665 ) ) ;
#13395 = VERTEX_POINT ( 'NONE', #5111 ) ;
#13396 = CARTESIAN_POINT ( 'NONE',  ( -1.346194077712558945, 0.5625000000000003331, -0.2500000000000002220 ) ) ;
#13397 = ORIENTED_EDGE ( 'NONE', *, *, #8752, .F. ) ;
#13398 = DIRECTION ( 'NONE',  ( 0.000000000000000000, -1.000000000000000000, 0.000000000000000000 ) ) ;
#13399 = CARTESIAN_POINT ( 'NONE',  ( -13.61615722309449872, 4.488109077202681521E-13, -189.4575979531706480 ) ) ;
#13400 = CARTESIAN_POINT ( 'NONE',  ( 1.553300858899105963, 8.562500000000001776, -7.250000000000000888 ) ) ;
#13401 = CARTESIAN_POINT ( 'NONE',  ( -2.651650429449552870, 6.875000000000000000, -6.151650429449552426 ) ) ;
#13402 = DIRECTION ( 'NONE',  ( 0.9997619372588932851, -0.000000000000000000, 0.02181900108494707474 ) ) ;
#13403 = VERTEX_POINT ( 'NONE', #13156 ) ;
#13404 = APPROVAL_PERSON_ORGANIZATION ( #7612, #15024, #7917 ) ;
#13405 = CARTESIAN_POINT ( 'NONE',  ( -9.079473912027703264, 3.253592935839261013, -115.4940425210697441 ) ) ;
#13406 = CARTESIAN_POINT ( 'NONE',  ( -2.298097038856279362, 4.875000000000000000, -5.798097038856278473 ) ) ;
#13407 = EDGE_CURVE ( 'NONE', #10375, #2594, #11449, .T. ) ;
#13408 = CARTESIAN_POINT ( 'NONE',  ( 3.750000000000000000, 10.75000000000000000, -3.500000000000000444 ) ) ;
#13409 = CARTESIAN_POINT ( 'NONE',  ( -69.61556017099954374, 14.99999999999885425, -198.3353672693050385 ) ) ;
#13410 = ADVANCED_FACE ( 'NONE', ( #3096 ), #4484, .T. ) ;
#13411 = ADVANCED_FACE ( 'NONE', ( #8326 ), #14478, .T. ) ;
#13412 = DIRECTION ( 'NONE',  ( 0.000000000000000000, 0.000000000000000000, 1.000000000000000000 ) ) ;
#13413 = DIRECTION ( 'NONE',  ( 0.6684085102769072861, 0.000000000000000000, -0.7437943690223837168 ) ) ;
#13414 = CARTESIAN_POINT ( 'NONE',  ( 2.298097038856279362, 7.875000000000000000, -1.201902961143720860 ) ) ;
#13415 = CARTESIAN_POINT ( 'NONE',  ( -4.406415408179883642, 15.00000000000000355, -116.9422405828140654 ) ) ;
#13416 = CARTESIAN_POINT ( 'NONE',  ( -9.518035002864159821, -1.966966232440479402E-12, -117.2217326882803832 ) ) ;
#13417 = CARTESIAN_POINT ( 'NONE',  ( 3.327290866796126068, 1.734723475976807094E-15, -114.7643839154946761 ) ) ;
#13418 = EDGE_LOOP ( 'NONE', ( #15054, #15262, #7851, #1174 ) ) ;
#13419 = CC_DESIGN_PERSON_AND_ORGANIZATION_ASSIGNMENT ( #3757, #6232, ( #12333 ) ) ;
#13420 = DIRECTION ( 'NONE',  ( 0.9961255586397056438, 0.000000000000000000, -0.08794243244722427244 ) ) ;
#13421 = CARTESIAN_POINT ( 'NONE',  ( 10.01939027896081313, 9.999999999999998224, -127.6977514918621637 ) ) ;
#13422 = ORIENTED_EDGE ( 'NONE', *, *, #13384, .T. ) ;
#13423 = VERTEX_POINT ( 'NONE', #8487 ) ;
#13424 = DIRECTION ( 'NONE',  ( 0.000000000000000000, 1.000000000000000000, 0.000000000000000000 ) ) ;
#13425 = CARTESIAN_POINT ( 'NONE',  ( 1.553300858899105963, 12.06250000000000000, -7.249999999999999112 ) ) ;
#13426 = AXIS2_PLACEMENT_3D ( 'NONE', #10194, #4469, #7794 ) ;
#13427 = CARTESIAN_POINT ( 'NONE',  ( -1.346194077712559167, 12.93750000000000178, -6.749999999999999112 ) ) ;
#13428 = CARTESIAN_POINT ( 'NONE',  ( 1.346194077712561166, 11.43750000000000178, -0.2500000000000011102 ) ) ;
#13429 = ORIENTED_EDGE ( 'NONE', *, *, #4220, .T. ) ;
#13430 = CARTESIAN_POINT ( 'NONE',  ( -0.9685250182442692868, 15.00000000000000000, -114.0968640496209190 ) ) ;
#13431 = CARTESIAN_POINT ( 'NONE',  ( 1.346194077712560944, 8.937500000000001776, -0.2500000000000010547 ) ) ;
#13432 = DIRECTION ( 'NONE',  ( 0.000000000000000000, 0.000000000000000000, 1.000000000000000000 ) ) ;
#13433 = FACE_OUTER_BOUND ( 'NONE', #6442, .T. ) ;
#13434 = CARTESIAN_POINT ( 'NONE',  ( -25.82983890416511841, 15.00000000000000000, -142.4527639562402328 ) ) ;
#13435 = DIRECTION ( 'NONE',  ( 0.000000000000000000, 0.000000000000000000, 1.000000000000000000 ) ) ;
#13436 = CIRCLE ( 'NONE', #3791, 2.500000000000000888 ) ;
#13437 = APPLICATION_PROTOCOL_DEFINITION ( 'international standard', 'config_control_design', 1994, #590 ) ;
#13438 = PLANE ( 'NONE',  #6018 ) ;
#13439 = EDGE_LOOP ( 'NONE', ( #187, #5760, #5509, #9521, #6949 ) ) ;
#13440 = CARTESIAN_POINT ( 'NONE',  ( 0.000000000000000000, 2.000000000000000000, -0.2500000000000002220 ) ) ;
#13441 = CARTESIAN_POINT ( 'NONE',  ( -3.749999999999999556, 13.18749999999999822, -1.946699141100892927 ) ) ;
#13442 = EDGE_LOOP ( 'NONE', ( #8101, #345, #1523, #8704 ) ) ;
#13443 = CARTESIAN_POINT ( 'NONE',  ( 10.97171279554003043, 8.773889247172311556, -44.61149169061435060 ) ) ;
#13444 = CIRCLE ( 'NONE', #8239, 1.000000000000000888 ) ;
#13445 = AXIS2_PLACEMENT_3D ( 'NONE', #1699, #4181, #472 ) ;
#13446 = CARTESIAN_POINT ( 'NONE',  ( 1.553300858899108849, 0.9374999999999998890, 0.2499999999999993616 ) ) ;
#13447 = DIRECTION ( 'NONE',  ( 0.000000000000000000, -1.000000000000000000, 0.000000000000000000 ) ) ;
#13448 = CARTESIAN_POINT ( 'NONE',  ( 13.87268740824488411, 13.20263832612636179, -126.2495228518582593 ) ) ;
#13449 = COORDINATED_UNIVERSAL_TIME_OFFSET ( 0, 0, .AHEAD. ) ;
#13450 = CARTESIAN_POINT ( 'NONE',  ( -67.63669501819022400, 12.89019592428436845, -202.2218604853389934 ) ) ;
#13451 = VECTOR ( 'NONE', #7541, 999.9999999999998863 ) ;
#13452 = DIRECTION ( 'NONE',  ( -0.000000000000000000, 1.000000000000000000, -0.000000000000000000 ) ) ;
#13453 = ORIENTED_EDGE ( 'NONE', *, *, #10521, .T. ) ;
#13454 = CARTESIAN_POINT ( 'NONE',  ( 2.298097038856278473, 8.625000000000000000, -5.798097038856279362 ) ) ;
#13455 = DIRECTION ( 'NONE',  ( -0.08794243244722436958, 0.000000000000000000, -0.9961255586397055328 ) ) ;
#13456 = CARTESIAN_POINT ( 'NONE',  ( -2.298097038856278918, 14.37500000000000000, -5.798097038856277585 ) ) ;
#13457 = CARTESIAN_POINT ( 'NONE',  ( 3.249999999999999556, 9.249999999999998224, -3.500000000000000000 ) ) ;
#13458 = CARTESIAN_POINT ( 'NONE',  ( -0.8684534520279955094, 10.00000000000000355, -104.6281219612548625 ) ) ;
#13459 = DIRECTION ( 'NONE',  ( 0.5024920151648527566, -0.000000000000000000, 0.8645818496218652394 ) ) ;
#13460 = CARTESIAN_POINT ( 'NONE',  ( 3.890350893699055401, 5.000000000000000000, -1.782295516753907849 ) ) ;
#13461 = CARTESIAN_POINT ( 'NONE',  ( 0.000000000000000000, 4.000000000000000000, -0.2500000000000002220 ) ) ;
#13462 = VECTOR ( 'NONE', #6744, 1000.000000000000000 ) ;
#13463 = CARTESIAN_POINT ( 'NONE',  ( 0.000000000000000000, 6.500000000000000000, 0.2499999999999998057 ) ) ;
#13464 = CARTESIAN_POINT ( 'NONE',  ( 2.651650429449553759, 9.875000000000000000, -0.8483495705504471296 ) ) ;
#13465 = DIRECTION ( 'NONE',  ( 0.02032500363963561651, 0.3636704086172907746, -0.9313059261720509907 ) ) ;
#13466 = CARTESIAN_POINT ( 'NONE',  ( -3.803734620756425322, 11.03678359822948885, -44.30700079492977039 ) ) ;
#13467 = CARTESIAN_POINT ( 'NONE',  ( -2.651650429449552870, 10.62500000000000000, -0.8483495705504463524 ) ) ;
#13468 = DIRECTION ( 'NONE',  ( -0.02181900108494707127, -0.000000000000000000, 0.9997619372588931741 ) ) ;
#13469 = CARTESIAN_POINT ( 'NONE',  ( 9.962419064811388836, 0.09217387118650985367, -163.9266138299434772 ) ) ;
#13470 = CARTESIAN_POINT ( 'NONE',  ( 11.91826453496365623, 0.000000000000000000, 18.75693026131819963 ) ) ;
#13471 = CARTESIAN_POINT ( 'NONE',  ( -30.34667403426979604, 4.000000000000237144, -197.7357094718530846 ) ) ;
#13472 = CARTESIAN_POINT ( 'NONE',  ( -0.3766621274091725424, 0.2144981952514214973, -6.953972463291595574 ) ) ;
#13473 = ADVANCED_FACE ( 'NONE', ( #10886 ), #10803, .T. ) ;
#13474 = CARTESIAN_POINT ( 'NONE',  ( 4.999884908348398049, 0.09438068890155060231, -1.653151978968578462 ) ) ;
#13475 = EDGE_CURVE ( 'NONE', #6134, #4565, #14218, .T. ) ;
#13476 = CARTESIAN_POINT ( 'NONE',  ( 3.749999999999999112, 14.18750000000000178, -5.053300858899108405 ) ) ;
#13477 = VERTEX_POINT ( 'NONE', #12348 ) ;
#13478 = CYLINDRICAL_SURFACE ( 'NONE', #13904, 2.000000000000001776 ) ;
#13479 = DIRECTION ( 'NONE',  ( 1.000000000000000000, 0.000000000000000000, 0.000000000000000000 ) ) ;
#13480 = CARTESIAN_POINT ( 'NONE',  ( -3.749999999999999556, 10.31250000000000000, -5.053300858899104853 ) ) ;
#13481 = CARTESIAN_POINT ( 'NONE',  ( 0.000000000000000000, 8.500000000000000000, 0.2499999999999998057 ) ) ;
#13482 = CARTESIAN_POINT ( 'NONE',  ( 27.03835354040200301, 6.000000000000000000, -138.2189567750508843 ) ) ;
#13483 = ORIENTED_EDGE ( 'NONE', *, *, #906, .F. ) ;
#13484 = CARTESIAN_POINT ( 'NONE',  ( -8.786545012119724163, 2.617545850260423190, -115.6253344005663166 ) ) ;
#13485 = CARTESIAN_POINT ( 'NONE',  ( 0.000000000000000000, 6.500000000000000000, -0.2500000000000002220 ) ) ;
#13486 = CARTESIAN_POINT ( 'NONE',  ( -3.749999999999999556, 14.18750000000000000, -1.946699141100892927 ) ) ;
#13487 =( BOUNDED_SURFACE ( )  B_SPLINE_SURFACE ( 3, 2, ( 
 ( #9691, #11997, #2583 ),
 ( #5058, #8763, #8522 ),
 ( #12240, #8444, #14656 ),
 ( #2741, #13256, #2661 ),
 ( #3821, #1346, #7444 ),
 ( #7362, #262, #9923 ),
 ( #9770, #8598, #12076 ),
 ( #1500, #4895, #3978 ),
 ( #3738, #14576, #6211 ),
 ( #13175, #7284, #10926 ),
 ( #3900, #14336, #4973 ),
 ( #13333, #14422, #9607 ),
 ( #12161, #1423, #9843 ),
 ( #343, #14501, #2819 ),
 ( #8682, #7521, #1576 ),
 ( #6291, #11007, #421 ),
 ( #5131, #13416, #2892 ),
 ( #184, #4059, #1651 ) ),
 .UNSPECIFIED., .F., .F., .T. ) 
 B_SPLINE_SURFACE_WITH_KNOTS ( ( 4, 2, 2, 2, 2, 2, 2, 2, 4 ),
 ( 3, 3 ),
 ( 0.000000000000000000, 0.002730992342634833061, 0.005461984685269666122, 0.008192977027904498749, 0.01092396937053933224, 0.01365496171317416574, 0.01638595405580899750, 0.01911694639844382926, 0.02184793874107866449 ),
 ( 0.000000000000000000, 1.000000000000000000 ),
 .UNSPECIFIED. ) 
 GEOMETRIC_REPRESENTATION_ITEM ( )  RATIONAL_B_SPLINE_SURFACE ( (
 ( 1.000000000000000000, 0.7071067811865475727, 1.000000000000000000),
 ( 1.000000000000000000, 0.7071067811865475727, 1.000000000000000000),
 ( 1.000000000000000000, 0.7071067811865475727, 1.000000000000000000),
 ( 1.000000000000000000, 0.7071067811865475727, 1.000000000000000000),
 ( 1.000000000000000000, 0.7071067811865476838, 1.000000000000000000),
 ( 1.000000000000000000, 0.7071067811865476838, 1.000000000000000000),
 ( 1.000000000000000000, 0.7071067811865473507, 1.000000000000000000),
 ( 1.000000000000000000, 0.7071067811865473507, 1.000000000000000000),
 ( 1.000000000000000000, 0.7071067811865476838, 1.000000000000000000),
 ( 1.000000000000000000, 0.7071067811865476838, 1.000000000000000000),
 ( 1.000000000000000000, 0.7071067811865471286, 1.000000000000000000),
 ( 1.000000000000000000, 0.7071067811865471286, 1.000000000000000000),
 ( 1.000000000000000000, 0.7071067811865477948, 1.000000000000000000),
 ( 1.000000000000000000, 0.7071067811865477948, 1.000000000000000000),
 ( 1.000000000000000000, 0.7071067811865477948, 1.000000000000000000),
 ( 1.000000000000000000, 0.7071067811865477948, 1.000000000000000000),
 ( 1.000000000000000000, 0.7071067811865476838, 1.000000000000000000),
 ( 1.000000000000000000, 0.7071067811865476838, 1.000000000000000000) ) ) 
 REPRESENTATION_ITEM ( '' )  SURFACE ( )  );
#13488 = PLANE ( 'NONE',  #9904 ) ;
#13489 = CARTESIAN_POINT ( 'NONE',  ( -7.439587717305479408, 0.000000000000000000, -35.49614290395457772 ) ) ;
#13490 = PERSON_AND_ORGANIZATION ( #3176, #3020 ) ;
#13491 = CARTESIAN_POINT ( 'NONE',  ( -3.249999999999999556, 11.18749999999999822, -2.153805922287440833 ) ) ;
#13492 = DIRECTION ( 'NONE',  ( -0.000000000000000000, -1.000000000000000000, -0.000000000000000000 ) ) ;
#13493 = DIRECTION ( 'NONE',  ( 0.000000000000000000, 0.000000000000000000, 1.000000000000000000 ) ) ;
#13494 = CARTESIAN_POINT ( 'NONE',  ( 10.27157762096145710, 5.000000000000000888, -107.9972514638527912 ) ) ;
#13495 = CARTESIAN_POINT ( 'NONE',  ( 0.000000000000000000, 15.00000000000000000, -100.6237003951525679 ) ) ;
#13496 = DIRECTION ( 'NONE',  ( 0.000000000000000000, 0.000000000000000000, -1.000000000000000000 ) ) ;
#13497 = B_SPLINE_CURVE_WITH_KNOTS ( 'NONE', 3,
 ( #2871, #4333, #9037, #5705, #3235, #11727, #4628, #10339, #15305, #994, #8026, #9265, #15082, #4476, #3316, #8172, #7013, #12823, #3539, #9186, #6719, #12591, #13989, #14062, #12667, #11577, #2008, #10424, #12900, #4557 ),
 .UNSPECIFIED., .F., .F.,
 ( 4, 2, 2, 2, 2, 2, 2, 2, 2, 2, 2, 2, 2, 2, 4 ),
 ( 2.602085213965210642E-18, 0.003534236666671877487, 0.004417795833339854122, 0.005301355000007830325, 0.007068473333343742830, 0.007952032500011699950, 0.008835591666679656203, 0.01060271000001552708, 0.01236982833335139795, 0.01413694666668726882, 0.01767118333335897587, 0.01943830166669482593, 0.02120542000003067598, 0.02473965666670241773, 0.02827389333337415600 ),
 .UNSPECIFIED. ) ;
#13498 = VERTEX_POINT ( 'NONE', #6554 ) ;
#13499 = EDGE_CURVE ( 'NONE', #14034, #14091, #1512, .T. ) ;
#13500 = CARTESIAN_POINT ( 'NONE',  ( 8.987149773678774878, 12.49999999999999645, 0.4909659112279870508 ) ) ;
#13501 = CARTESIAN_POINT ( 'NONE',  ( 25.28120514378732864, 1.499740039320041296, -138.4427521360613866 ) ) ;
#13502 = CARTESIAN_POINT ( 'NONE',  ( 3.749999999999998668, 13.18750000000000000, -5.053300858899108405 ) ) ;
#13503 = CARTESIAN_POINT ( 'NONE',  ( 0.000000000000000000, 11.50000000000000000, -0.2500000000000002220 ) ) ;
#13504 = ADVANCED_FACE ( 'NONE', ( #11266 ), #6399, .F. ) ;
#13505 = CARTESIAN_POINT ( 'NONE',  ( 3.249999999999999556, 1.750000000000000000, -3.500000000000000000 ) ) ;
#13506 = ORIENTED_EDGE ( 'NONE', *, *, #3452, .T. ) ;
#13507 = CARTESIAN_POINT ( 'NONE',  ( 1.346194077712560944, 12.93750000000000000, -0.2500000000000010547 ) ) ;
#13508 = DIRECTION ( 'NONE',  ( 0.000000000000000000, 1.000000000000000000, 0.000000000000000000 ) ) ;
#13509 = CARTESIAN_POINT ( 'NONE',  ( -6.243492141569531917, 14.55944995895985450, -103.9608192963590625 ) ) ;
#13510 = CARTESIAN_POINT ( 'NONE',  ( -24.82368063746440612, 4.000000000000000000, -209.1616663288132827 ) ) ;
#13511 = CARTESIAN_POINT ( 'NONE',  ( -57.52695389842154583, 14.99999999999999822, -167.0767265278727791 ) ) ;
#13512 = SHAPE_DEFINITION_REPRESENTATION ( #4478, #7636 ) ;
#13513 = CARTESIAN_POINT ( 'NONE',  ( 12.44913988807079086, 15.00000000000000000, -128.2750425511075036 ) ) ;
#13514 = ORIENTED_EDGE ( 'NONE', *, *, #8286, .T. ) ;
#13515 = CARTESIAN_POINT ( 'NONE',  ( -3.249999999999999556, 1.312500000000000444, -4.846194077712557835 ) ) ;
#13516 = CARTESIAN_POINT ( 'NONE',  ( -4.592425496802573972E-16, 12.50000000000000000, -7.249999999999999112 ) ) ;
#13517 = EDGE_CURVE ( 'NONE', #13758, #14016, #8905, .T. ) ;
#13518 = ORIENTED_EDGE ( 'NONE', *, *, #1168, .F. ) ;
#13519 = CARTESIAN_POINT ( 'NONE',  ( -10.29275726619092524, -1.020558061026469066, -34.56909192082969184 ) ) ;
#13520 = B_SPLINE_CURVE_WITH_KNOTS ( 'NONE', 3,
 ( #6230, #10944, #362, #3917, #1743, #739, #2980, #13728, #10166, #667, #592, #3055, #6453, #7609, #3128, #14900, #8926, #6379, #12402, #9938, #8781, #6685 ),
 .UNSPECIFIED., .F., .F.,
 ( 4, 2, 2, 2, 2, 2, 2, 2, 2, 2, 4 ),
 ( 0.000000000000000000, 0.001234958623131101165, 0.002469917246262202330, 0.003704875869393304145, 0.004322355180958854619, 0.004939834492524404659, 0.005557313804089955567, 0.006174793115655505607, 0.007409751738786608290, 0.008644710361917709238, 0.009879668985048807583 ),
 .UNSPECIFIED. ) ;
#13521 = CARTESIAN_POINT ( 'NONE',  ( -1.553300858899107295, 2.437500000000000444, -7.250000000000000000 ) ) ;
#13522 = DIRECTION ( 'NONE',  ( -0.000000000000000000, 1.000000000000000000, -0.000000000000000000 ) ) ;
#13523 = CARTESIAN_POINT ( 'NONE',  ( 0.2508056121593058019, 4.191234989200504302, 2.840879807056750472 ) ) ;
#13524 = CARTESIAN_POINT ( 'NONE',  ( 7.434948248173551377, 5.000000000000000888, -26.28946758364566705 ) ) ;
#13525 = APPROVAL_STATUS ( 'not_yet_approved' ) ;
#13526 = CARTESIAN_POINT ( 'NONE',  ( -67.09168088980882771, 14.54755436366324695, -195.2977458324043596 ) ) ;
#13527 = CARTESIAN_POINT ( 'NONE',  ( 2.850044070969222521, 15.00000000000000000, -103.0233998225063345 ) ) ;
#13528 = ORIENTED_EDGE ( 'NONE', *, *, #5451, .F. ) ;
#13529 = CARTESIAN_POINT ( 'NONE',  ( -3.249999999999999556, 9.312500000000000000, -4.846194077712557835 ) ) ;
#13530 = DIRECTION ( 'NONE',  ( 0.9961255586397056438, 0.000000000000000000, -0.08794243244722427244 ) ) ;
#13531 = CARTESIAN_POINT ( 'NONE',  ( -3.249999999999999556, 4.750000000000000000, -3.500000000000000000 ) ) ;
#13532 = CARTESIAN_POINT ( 'NONE',  ( 1.346194077712561166, 11.43750000000000178, -0.2500000000000011102 ) ) ;
#13533 = DIRECTION ( 'NONE',  ( -0.08794243244723005948, -0.000000000000000000, -0.9961255586397049777 ) ) ;
#13534 = CARTESIAN_POINT ( 'NONE',  ( -8.818042780597295405, 4.336808689942017736E-16, -127.1624902446298364 ) ) ;
#13535 = CARTESIAN_POINT ( 'NONE',  ( -2.298097038856278473, 6.125000000000000000, -1.201902961143720416 ) ) ;
#13536 = CARTESIAN_POINT ( 'NONE',  ( -3.750000000000000000, 3.812500000000000000, -5.053300858899105741 ) ) ;
#13537 = CARTESIAN_POINT ( 'NONE',  ( 3.749999999999999112, 8.687500000000000000, -5.053300858899108405 ) ) ;
#13538 = CARTESIAN_POINT ( 'NONE',  ( 0.01496453197139708223, 0.000000000000000000, 5.196130874293197088 ) ) ;
#13539 = CARTESIAN_POINT ( 'NONE',  ( -9.410661088365667837, 3.301239252470002050, -116.4362230898866528 ) ) ;
#13540 = CARTESIAN_POINT ( 'NONE',  ( -4.592425496802573972E-16, 11.00000000000000000, -7.250000000000000000 ) ) ;
#13541 = CARTESIAN_POINT ( 'NONE',  ( -25.82983890416511841, 9.999999999999998224, -157.2527639562405000 ) ) ;
#13542 = CARTESIAN_POINT ( 'NONE',  ( 12.73470083568815170, 2.902482184389665765, -166.2121014961018375 ) ) ;
#13543 = CARTESIAN_POINT ( 'NONE',  ( 10.89041330322193701, 3.672903760508912097, -107.0396867723672329 ) ) ;
#13544 = CARTESIAN_POINT ( 'NONE',  ( -15.97579411175272313, 3.999999999999753975, -155.0504951762476082 ) ) ;
#13545 = DIRECTION ( 'NONE',  ( 0.003262051938530752433, 0.000000000000000000, 0.9999946794944213346 ) ) ;
#13546 = CARTESIAN_POINT ( 'NONE',  ( -44.82692087594050179, 15.00000000000000000, -154.1244306586370101 ) ) ;
#13547 = CARTESIAN_POINT ( 'NONE',  ( -3.750000000000000000, 13.68750000000000178, -1.946699141100893149 ) ) ;
#13548 = ORIENTED_EDGE ( 'NONE', *, *, #8852, .T. ) ;
#13549 = CARTESIAN_POINT ( 'NONE',  ( 10.99340860758277927, 5.943472311793079221, -45.60560901953395785 ) ) ;
#13550 = CARTESIAN_POINT ( 'NONE',  ( 16.61630038475162863, 8.673617379884034486E-16, -146.8898935758374478 ) ) ;
#13551 = CARTESIAN_POINT ( 'NONE',  ( 2.651650429449553314, 8.375000000000000000, -0.8483495705504476847 ) ) ;
#13552 = CARTESIAN_POINT ( 'NONE',  ( -3.395817407829019530, 10.62992890784805766, -45.78935231847124498 ) ) ;
#13553 = CARTESIAN_POINT ( 'NONE',  ( -1.346194077712559167, 6.937500000000001776, -6.749999999999999112 ) ) ;
#13554 = CARTESIAN_POINT ( 'NONE',  ( 3.749999999999999556, 0.2500000000000001110, -3.500000000000000444 ) ) ;
#13555 = DIRECTION ( 'NONE',  ( 0.000000000000000000, 0.000000000000000000, -1.000000000000000000 ) ) ;
#13556 = CYLINDRICAL_SURFACE ( 'NONE', #1233, 3.187847681061608540 ) ;
#13557 = EDGE_CURVE ( 'NONE', #4119, #14756, #10385, .T. ) ;
#13558 = CALENDAR_DATE ( 2026, 8, 10 ) ;
#13559 = CARTESIAN_POINT ( 'NONE',  ( -3.980102097228897245E-16, 11.50000000000000000, -6.749999999999999112 ) ) ;
#13560 = CARTESIAN_POINT ( 'NONE',  ( -0.3766621274091715987, -0.2500000000000000000, -6.863050255469941519 ) ) ;
#13561 = DIRECTION ( 'NONE',  ( 0.000000000000000000, 0.000000000000000000, 1.000000000000000000 ) ) ;
#13562 = CARTESIAN_POINT ( 'NONE',  ( 9.112041370335649759, -1.070315399344735426E-12, -109.9899024349114853 ) ) ;
#13563 = CARTESIAN_POINT ( 'NONE',  ( -7.234633885585873614, 9.999999999999998224, -146.9955140158000404 ) ) ;
#13564 = CARTESIAN_POINT ( 'NONE',  ( -3.520407287333057855, 7.379999999999995453, -45.56125597433126018 ) ) ;
#13565 = ORIENTED_EDGE ( 'NONE', *, *, #8460, .T. ) ;
#13566 = CARTESIAN_POINT ( 'NONE',  ( 7.788671722263534214, 5.321094445766561876, -20.36947622874119546 ) ) ;
#13567 = CARTESIAN_POINT ( 'NONE',  ( -17.32624372123753886, 9.999999999999998224, -122.3796757791585321 ) ) ;
#13568 = CARTESIAN_POINT ( 'NONE',  ( 3.749999999999998668, 1.687500000000000000, -5.053300858899107517 ) ) ;
#13569 = CARTESIAN_POINT ( 'NONE',  ( 2.298097038856279362, 9.374999999999998224, -1.201902961143720860 ) ) ;
#13570 = CARTESIAN_POINT ( 'NONE',  ( 2.298097038856278473, 0.6250000000000000000, -5.798097038856279362 ) ) ;
#13571 = VERTEX_POINT ( 'NONE', #11193 ) ;
#13572 =( BOUNDED_SURFACE ( )  B_SPLINE_SURFACE ( 3, 1, ( 
 ( #11589, #6873 ),
 ( #11668, #4638 ),
 ( #8035, #4342 ),
 ( #3166, #2171 ) ),
 .UNSPECIFIED., .F., .F., .F. ) 
 B_SPLINE_SURFACE_WITH_KNOTS ( ( 4, 4 ),
 ( 2, 2 ),
 ( 0.000000000000000000, 1.000000000000000000 ),
 ( 0.000000000000000000, 1.000000000000000000 ),
 .UNSPECIFIED. ) 
 GEOMETRIC_REPRESENTATION_ITEM ( )  RATIONAL_B_SPLINE_SURFACE ( (
 ( 1.000000000000000000, 1.000000000000000000),
 ( 0.9863449930132133225, 0.9863449930132133225),
 ( 0.9863449930132133225, 0.9863449930132133225),
 ( 1.000000000000000000, 1.000000000000000000) ) ) 
 REPRESENTATION_ITEM ( '' )  SURFACE ( )  );
#13573 = CARTESIAN_POINT ( 'NONE',  ( -2.298097038856278918, 11.37500000000000000, -5.798097038856277585 ) ) ;
#13574 = CARTESIAN_POINT ( 'NONE',  ( -2.869987474717192732, -2.165641995260736863, -0.9999999999968022246 ) ) ;
#13575 = CARTESIAN_POINT ( 'NONE',  ( 9.940211158120405344, 12.49999999999999822, -43.17897536272747772 ) ) ;
#13576 = EDGE_CURVE ( 'NONE', #13038, #10677, #14848, .T. ) ;
#13577 = CARTESIAN_POINT ( 'NONE',  ( 0.3766621274091715987, 0.5000000000000000000, -7.146945437571387671 ) ) ;
#13578 = CARTESIAN_POINT ( 'NONE',  ( -9.076832803613291034, 12.38245414981636650, -116.5147594324881339 ) ) ;
#13579 = EDGE_CURVE ( 'NONE', #12717, #14660, #7192, .T. ) ;
#13580 = CALENDAR_DATE ( 2026, 8, 10 ) ;
#13581 = CARTESIAN_POINT ( 'NONE',  ( 11.05697737868720232, 15.00000000000186162, -122.2826711086158014 ) ) ;
#13582 = ORIENTED_EDGE ( 'NONE', *, *, #3849, .T. ) ;
#13583 = CARTESIAN_POINT ( 'NONE',  ( 2.298097038856278473, 3.625000000000000000, -5.798097038856279362 ) ) ;
#13584 = DIRECTION ( 'NONE',  ( 0.000000000000000000, 0.000000000000000000, -1.000000000000000000 ) ) ;
#13585 = CARTESIAN_POINT ( 'NONE',  ( -1.553300858899106629, 12.06250000000000000, 0.2500000000000002220 ) ) ;
#13586 = ORIENTED_EDGE ( 'NONE', *, *, #11695, .T. ) ;
#13587 = LOCAL_TIME ( 12, 28, 20.00000000000000000, #11644 ) ;
#13588 = CARTESIAN_POINT ( 'NONE',  ( 6.422699671861707316, 6.000000000000000000, -139.1645012375703061 ) ) ;
#13589 = VECTOR ( 'NONE', #12639, 1000.000000000000114 ) ;
#13590 = EDGE_CURVE ( 'NONE', #6698, #6397, #5322, .T. ) ;
#13591 = CARTESIAN_POINT ( 'NONE',  ( 3.749999999999999112, 1.812500000000000222, -1.946699141100892039 ) ) ;
#13592 = CARTESIAN_POINT ( 'NONE',  ( -67.58382170693636226, 9.999999999999998224, -204.5178482451962623 ) ) ;
#13593 = EDGE_CURVE ( 'NONE', #2743, #7043, #14852, .T. ) ;
#13594 = CARTESIAN_POINT ( 'NONE',  ( 0.09748540496241393793, 2.577905345474640342, 1.104218984803364778 ) ) ;
#13595 = CARTESIAN_POINT ( 'NONE',  ( 11.04730217088330413, 5.000000000000001776, -107.1178495010084504 ) ) ;
#13596 = EDGE_CURVE ( 'NONE', #4779, #12117, #14099, .T. ) ;
#13597 = PERSON_AND_ORGANIZATION ( #3176, #3020 ) ;
#13598 = EDGE_CURVE ( 'NONE', #5201, #2826, #9401, .T. ) ;
#13599 = ORIENTED_EDGE ( 'NONE', *, *, #3097, .F. ) ;
#13600 = CARTESIAN_POINT ( 'NONE',  ( -67.59778896351508592, 11.06839609948164060, -204.2590688364760467 ) ) ;
#13601 = FACE_OUTER_BOUND ( 'NONE', #5546, .T. ) ;
#13602 = CIRCLE ( 'NONE', #1984, 3.000000000000000000 ) ;
#13603 = ORIENTED_EDGE ( 'NONE', *, *, #2737, .T. ) ;
#13604 = CARTESIAN_POINT ( 'NONE',  ( -0.3766621274091715987, 0.5000000000000000000, -6.863050255469941519 ) ) ;
#13605 = CARTESIAN_POINT ( 'NONE',  ( -1.346194077712559167, 2.937500000000000444, -6.749999999999999112 ) ) ;
#13606 = CARTESIAN_POINT ( 'NONE',  ( -3.980102097228897738E-16, 11.00000000000000000, -6.749999999999999112 ) ) ;
#13607 = CARTESIAN_POINT ( 'NONE',  ( -4.116580123655899648E-16, 10.00000000000000000, -101.3854116612075700 ) ) ;
#13608 = AXIS2_PLACEMENT_3D ( 'NONE', #14013, #6886, #4581 ) ;
#13609 = CARTESIAN_POINT ( 'NONE',  ( 1.203323408085149371, 4.317064434386042038, -139.4038898281761760 ) ) ;
#13610 = CARTESIAN_POINT ( 'NONE',  ( 3.249999999999999112, 4.812500000000000888, -2.153805922287439945 ) ) ;
#13611 = CARTESIAN_POINT ( 'NONE',  ( 3.749999999999998668, 4.187500000000000888, -5.053300858899108405 ) ) ;
#13612 = VECTOR ( 'NONE', #12510, 1000.000000000000000 ) ;
#13613 = CARTESIAN_POINT ( 'NONE',  ( -3.750000000000000000, 9.187500000000000000, -1.946699141100892927 ) ) ;
#13614 = CARTESIAN_POINT ( 'NONE',  ( 0.000000000000000000, 0.000000000000000000, 0.000000000000000000 ) ) ;
#13615 = ORIENTED_EDGE ( 'NONE', *, *, #5993, .T. ) ;
#13616 = CARTESIAN_POINT ( 'NONE',  ( -3.842608339013799057, 9.819420005877756097, -43.36399912072333507 ) ) ;
#13617 = CARTESIAN_POINT ( 'NONE',  ( -3.750000000000000000, 8.687499999999998224, -1.946699141100893149 ) ) ;
#13618 = CARTESIAN_POINT ( 'NONE',  ( 4.999884908348399826, 0.09438068890153285262, -1.653151978968515845 ) ) ;
#13619 = CARTESIAN_POINT ( 'NONE',  ( 8.935548306746154523, 5.000000000000000888, 2.855381328098136162 ) ) ;
#13620 = CARTESIAN_POINT ( 'NONE',  ( 6.914202122640618953, 1.078315293502086643E-12, -105.2584297683565211 ) ) ;
#13621 = CC_DESIGN_PERSON_AND_ORGANIZATION_ASSIGNMENT ( #2381, #7079, ( #8304 ) ) ;
#13622 = CARTESIAN_POINT ( 'NONE',  ( -29.87892995173857003, 3.999999999999993783, -184.6141453219341599 ) ) ;
#13623 = CARTESIAN_POINT ( 'NONE',  ( 3.249999999999999556, 0.7500000000000000000, -3.500000000000000000 ) ) ;
#13624 = UNCERTAINTY_MEASURE_WITH_UNIT (LENGTH_MEASURE( 1.000000000000000082E-05 ), #892, 'distance_accuracy_value', 'NONE');
#13625 = CARTESIAN_POINT ( 'NONE',  ( -28.38930394846588001, 15.00000000000000000, -151.9126338648069066 ) ) ;
#13626 = CARTESIAN_POINT ( 'NONE',  ( -2.298097038856278029, -0.3749999999999998890, -1.201902961143720638 ) ) ;
#13627 = ORIENTED_EDGE ( 'NONE', *, *, #7824, .F. ) ;
#13628 = DIRECTION ( 'NONE',  ( 0.07380050482453413829, -0.002800241259227994727, 0.9972690931421338556 ) ) ;
#13629 = CARTESIAN_POINT ( 'NONE',  ( 11.05182978094480895, 3.355895706359027564, -106.3279719483364829 ) ) ;
#13630 = LINE ( 'NONE', #2806, #10455 ) ;
#13631 = CARTESIAN_POINT ( 'NONE',  ( -3.249999999999999112, 8.812500000000001776, -4.846194077712558723 ) ) ;
#13632 = CARTESIAN_POINT ( 'NONE',  ( 10.01939027896081313, 5.000000000000000888, -127.6977514918621637 ) ) ;
#13633 = CARTESIAN_POINT ( 'NONE',  ( -2.651650429449553314, 12.37500000000000000, -6.151650429449552426 ) ) ;
#13634 = CARTESIAN_POINT ( 'NONE',  ( -68.36774365772026840, 9.999999999999998224, -202.8408623589480442 ) ) ;
#13635 = FACE_OUTER_BOUND ( 'NONE', #4402, .T. ) ;
#13636 = CARTESIAN_POINT ( 'NONE',  ( 0.000000000000000000, 13.00000000000000178, -0.2500000000000002220 ) ) ;
#13637 = FACE_OUTER_BOUND ( 'NONE', #13021, .T. ) ;
#13638 = LINE ( 'NONE', #10227, #13462 ) ;
#13639 = CARTESIAN_POINT ( 'NONE',  ( -1.346194077712559389, 7.062500000000000000, -0.2500000000000002220 ) ) ;
#13640 = CARTESIAN_POINT ( 'NONE',  ( -16.94138229547579400, 9.999999999999998224, -154.2864167784019287 ) ) ;
#13641 = CARTESIAN_POINT ( 'NONE',  ( 8.881449363785039353, 9.999999999999998224, -2.080517014814270205 ) ) ;
#13642 = CC_DESIGN_SECURITY_CLASSIFICATION ( #7950, ( #10417 ) ) ;
#13643 = VERTEX_POINT ( 'NONE', #13751 ) ;
#13644 = CARTESIAN_POINT ( 'NONE',  ( 8.935548306746158076, 10.33196145731881721, 2.855381328098129057 ) ) ;
#13645 = CARTESIAN_POINT ( 'NONE',  ( -14.95313816010867392, 3.999999999999999112, -192.4638183655883097 ) ) ;
#13646 = CARTESIAN_POINT ( 'NONE',  ( 1.553300858899108849, 2.937500000000000444, 0.2499999999999993616 ) ) ;
#13647 = CARTESIAN_POINT ( 'NONE',  ( -3.249999999999999556, 14.75000000000000000, -3.500000000000000000 ) ) ;
#13648 = CARTESIAN_POINT ( 'NONE',  ( -1.346194077712559167, 12.93750000000000178, -6.749999999999999112 ) ) ;
#13649 = ORIENTED_EDGE ( 'NONE', *, *, #14414, .F. ) ;
#13650 = CARTESIAN_POINT ( 'NONE',  ( -3.980102097228897245E-16, 11.50000000000000000, -6.749999999999999112 ) ) ;
#13651 = CARTESIAN_POINT ( 'NONE',  ( 10.04032073682954618, 11.75496761609937657, -45.01598776155166348 ) ) ;
#13652 = B_SPLINE_CURVE_WITH_KNOTS ( 'NONE', 3,
 ( #13771, #9198, #12602, #15173, #4566, #5638, #2093, #10512, #9348, #15017 ),
 .UNSPECIFIED., .F., .F.,
 ( 4, 2, 2, 2, 4 ),
 ( 9.697399036122160616E-19, 0.0002702708960404995829, 0.0005405417920809981900, 0.0008108126881214967972, 0.001081083584161995296 ),
 .UNSPECIFIED. ) ;
#13653 = CC_DESIGN_APPROVAL ( #8931, ( #13898 ) ) ;
#13654 = CARTESIAN_POINT ( 'NONE',  ( 9.955014136429161553, 12.67960752135156888, -44.14371989070262003 ) ) ;
#13655 = PLANE ( 'NONE',  #9926 ) ;
#13656 = CARTESIAN_POINT ( 'NONE',  ( -8.207841483268280669, 13.21761715706680462, -115.8806436028953186 ) ) ;
#13657 = COORDINATED_UNIVERSAL_TIME_OFFSET ( 0, 0, .AHEAD. ) ;
#13658 = CARTESIAN_POINT ( 'NONE',  ( 11.32055997300887462, 12.49999999999999822, -122.6997364777432438 ) ) ;
#13659 = CIRCLE ( 'NONE', #2532, 1.000000000000028644 ) ;
#13660 = CARTESIAN_POINT ( 'NONE',  ( 27.03835354040196037, 5.000000000000001776, -138.2189567750509696 ) ) ;
#13661 = ORIENTED_EDGE ( 'NONE', *, *, #320, .T. ) ;
#13662 = CARTESIAN_POINT ( 'NONE',  ( 3.249999999999999556, 2.750000000000000000, -3.500000000000000000 ) ) ;
#13663 = CARTESIAN_POINT ( 'NONE',  ( 2.449293598294706414E-16, 0.000000000000000000, 2.000000000000000000 ) ) ;
#13664 = CARTESIAN_POINT ( 'NONE',  ( 3.749999999999999112, 3.187500000000000444, -5.053300858899108405 ) ) ;
#13665 = ORIENTED_EDGE ( 'NONE', *, *, #14917, .T. ) ;
#13666 = EDGE_CURVE ( 'NONE', #8297, #13794, #769, .T. ) ;
#13667 = DIRECTION ( 'NONE',  ( 0.08794243244723003172, 0.000000000000000000, 0.9961255586397049777 ) ) ;
#13668 = CARTESIAN_POINT ( 'NONE',  ( -4.592425496802573972E-16, 3.500000000000000000, -7.249999999999999112 ) ) ;
#13669 = VECTOR ( 'NONE', #2062, 1000.000000000000114 ) ;
#13670 = CARTESIAN_POINT ( 'NONE',  ( 7.229955861305157327, 3.179325318140356682, -23.98019230486299236 ) ) ;
#13671 = CARTESIAN_POINT ( 'NONE',  ( 2.653424689224152644, 0.03126846220630731532, 0.8711017884127576494 ) ) ;
#13672 = CARTESIAN_POINT ( 'NONE',  ( 1.553300858899108849, 1.937500000000000000, 0.2499999999999993616 ) ) ;
#13673 = CALENDAR_DATE ( 2026, 8, 10 ) ;
#13674 = PLANE ( 'NONE',  #4061 ) ;
#13675 = DIRECTION ( 'NONE',  ( 0.000000000000000000, 0.000000000000000000, 1.000000000000000000 ) ) ;
#13676 = VERTEX_POINT ( 'NONE', #8949 ) ;
#13677 = CIRCLE ( 'NONE', #15176, 0.5000000000000004441 ) ;
#13678 = CARTESIAN_POINT ( 'NONE',  ( -28.38930394846591909, 15.00000000000000000, -151.9126338648069918 ) ) ;
#13679 = VECTOR ( 'NONE', #12724, 1000.000000000000000 ) ;
#13680 = CARTESIAN_POINT ( 'NONE',  ( 2.298097038856278029, 3.125000000000000444, -5.798097038856279362 ) ) ;
#13681 = DIRECTION ( 'NONE',  ( 0.000000000000000000, 0.000000000000000000, 1.000000000000000000 ) ) ;
#13682 = EDGE_CURVE ( 'NONE', #10654, #9540, #14028, .T. ) ;
#13683 = EDGE_CURVE ( 'NONE', #13395, #11095, #10399, .T. ) ;
#13684 = CARTESIAN_POINT ( 'NONE',  ( -25.97807323962435078, 5.000000000000000000, -142.5647913107548277 ) ) ;
#13685 = CARTESIAN_POINT ( 'NONE',  ( 1.553300858899105963, 6.062500000000000000, -7.249999999999999112 ) ) ;
#13686 = CARTESIAN_POINT ( 'NONE',  ( 1.553300858899105963, 8.562500000000000000, -7.250000000000000000 ) ) ;
#13687 = CARTESIAN_POINT ( 'NONE',  ( 10.98638689276455871, 5.830414921909241599, -45.28386912034150669 ) ) ;
#13688 = LINE ( 'NONE', #3085, #14865 ) ;
#13689 = CARTESIAN_POINT ( 'NONE',  ( 3.750000000000000000, 10.31250000000000000, -1.946699141100892705 ) ) ;
#13690 = CIRCLE ( 'NONE', #5771, 7.000000000000000000 ) ;
#13691 = CARTESIAN_POINT ( 'NONE',  ( 1.004809442601927394, 6.000000000000000000, -139.4752805618705622 ) ) ;
#13692 = CARTESIAN_POINT ( 'NONE',  ( 6.095360508540255573, 15.00000000000000000, -116.7523417411930211 ) ) ;
#13693 = CARTESIAN_POINT ( 'NONE',  ( 3.230086961373113130, 5.000000000000000888, 5.208283729180105404 ) ) ;
#13694 = EDGE_LOOP ( 'NONE', ( #12801, #1249 ) ) ;
#13695 = CARTESIAN_POINT ( 'NONE',  ( -30.68313436375902370, 4.000000000000354383, -191.4730121854663878 ) ) ;
#13696 = DIRECTION ( 'NONE',  ( 0.000000000000000000, -1.000000000000000000, 0.000000000000000000 ) ) ;
#13697 = CARTESIAN_POINT ( 'NONE',  ( -34.35934156840468745, 9.999999999999998224, -156.1669470277516041 ) ) ;
#13698 = CARTESIAN_POINT ( 'NONE',  ( 1.346194077712561166, 3.437500000000000444, -0.2500000000000011102 ) ) ;
#13699 = ORIENTED_EDGE ( 'NONE', *, *, #11469, .F. ) ;
#13700 = DIRECTION ( 'NONE',  ( 0.000000000000000000, 0.000000000000000000, 1.000000000000000000 ) ) ;
#13701 = CARTESIAN_POINT ( 'NONE',  ( -0.4453226528549816265, -2.225540348348185052E-17, 1.000000000000000000 ) ) ;
#13702 = AXIS2_PLACEMENT_3D ( 'NONE', #11155, #15031, #4280 ) ;
#13703 = EDGE_CURVE ( 'NONE', #9868, #15191, #8674, .T. ) ;
#13704 = CARTESIAN_POINT ( 'NONE',  ( -3.589007869510364657, 10.29140990637095854, -47.02124496736357173 ) ) ;
#13705 = CARTESIAN_POINT ( 'NONE',  ( -16.87511749404491823, 8.673617379884032514E-16, -186.9742884131397318 ) ) ;
#13706 = CARTESIAN_POINT ( 'NONE',  ( -5.318033920936450443, 8.673617379884035472E-16, -111.4753907371134574 ) ) ;
#13707 = CARTESIAN_POINT ( 'NONE',  ( -2.298097038856278029, 9.624999999999998224, -1.201902961143720638 ) ) ;
#13708 = PLANE ( 'NONE',  #4000 ) ;
#13709 = CARTESIAN_POINT ( 'NONE',  ( 3.749999999999998668, 12.68750000000000178, -5.053300858899107517 ) ) ;
#13710 = CARTESIAN_POINT ( 'NONE',  ( -63.95352844018274396, 15.00000000000000000, -200.3649080088305539 ) ) ;
#13711 = CARTESIAN_POINT ( 'NONE',  ( -6.113022954200721060, 12.39308942777827127, -125.0150693682166292 ) ) ;
#13712 = CARTESIAN_POINT ( 'NONE',  ( -2.298097038856278918, 11.37500000000000000, -5.798097038856277585 ) ) ;
#13713 = LINE ( 'NONE', #13560, #1908 ) ;
#13714 = CARTESIAN_POINT ( 'NONE',  ( -17.32624372123753886, 15.00000000000000000, -129.3796757791584753 ) ) ;
#13715 = CARTESIAN_POINT ( 'NONE',  ( 3.249999999999999556, 7.750000000000000000, -3.500000000000000000 ) ) ;
#13716 = CARTESIAN_POINT ( 'NONE',  ( -1.500000000000000000, 4.500000000000000888, -0.2499999999999997780 ) ) ;
#13717 = DIRECTION ( 'NONE',  ( -0.000000000000000000, -1.000000000000000000, -0.000000000000000000 ) ) ;
#13718 = VERTEX_POINT ( 'NONE', #8615 ) ;
#13719 = CARTESIAN_POINT ( 'NONE',  ( 7.784015231764366938, 5.104710470816894663, -20.44740824490198960 ) ) ;
#13720 = CARTESIAN_POINT ( 'NONE',  ( -1.885039096047290252, 15.00000000000000178, -115.1740262261674985 ) ) ;
#13721 = CARTESIAN_POINT ( 'NONE',  ( 3.749999999999999112, 15.31250000000000355, -1.946699141100893149 ) ) ;
#13722 = CARTESIAN_POINT ( 'NONE',  ( -3.750000000000000000, 0.8124999999999997780, -5.053300858899105741 ) ) ;
#13723 = CARTESIAN_POINT ( 'NONE',  ( -2.298097038856278029, 13.62500000000000000, -1.201902961143720638 ) ) ;
#13724 = VERTEX_POINT ( 'NONE', #14358 ) ;
#13725 = CARTESIAN_POINT ( 'NONE',  ( -1.346194077712559389, 11.43750000000000000, -6.749999999999999112 ) ) ;
#13726 = LINE ( 'NONE', #1821, #11855 ) ;
#13727 = CARTESIAN_POINT ( 'NONE',  ( -8.963920885435754826, 11.76682784975604434, -105.0444811867494224 ) ) ;
#13728 = CARTESIAN_POINT ( 'NONE',  ( 4.543692464186339208, 0.6724431706707657552, 2.119679957923213731 ) ) ;
#13729 = CARTESIAN_POINT ( 'NONE',  ( -5.492028030077825917, 14.89159520566441408, -117.0085585369580770 ) ) ;
#13730 = APPROVAL_ROLE ( '' ) ;
#13731 = CARTESIAN_POINT ( 'NONE',  ( 6.454204466557374786, 15.00000000000000000, -118.3005150008459196 ) ) ;
#13732 = CARTESIAN_POINT ( 'NONE',  ( -4.234402844927150689, 15.00000000000000000, -117.4888040839639558 ) ) ;
#13733 = CARTESIAN_POINT ( 'NONE',  ( 22.20883717620709774, 0.09828479603275584731, -138.5096390345515545 ) ) ;
#13734 = EDGE_LOOP ( 'NONE', ( #2488, #5881, #14965, #444 ) ) ;
#13735 = CARTESIAN_POINT ( 'NONE',  ( -2.298097038856278918, 6.375000000000000888, -5.798097038856277585 ) ) ;
#13736 = CARTESIAN_POINT ( 'NONE',  ( -21.96202414993823382, 4.000000000000001776, -164.0357374456417006 ) ) ;
#13737 = CARTESIAN_POINT ( 'NONE',  ( -2.651650429449553314, -0.1249999999999999029, -6.151650429449552426 ) ) ;
#13738 = ORIENTED_EDGE ( 'NONE', *, *, #12494, .F. ) ;
#13739 = FACE_OUTER_BOUND ( 'NONE', #12783, .T. ) ;
#13740 = LINE ( 'NONE', #1542, #359 ) ;
#13741 = CARTESIAN_POINT ( 'NONE',  ( -3.750000000000000000, 7.250000000000000000, -3.499999999999999112 ) ) ;
#13742 = DIRECTION ( 'NONE',  ( 0.000000000000000000, 0.000000000000000000, 1.000000000000000000 ) ) ;
#13743 = DIRECTION ( 'NONE',  ( -0.000000000000000000, -1.000000000000000000, -0.000000000000000000 ) ) ;
#13744 = ADVANCED_FACE ( 'NONE', ( #441 ), #7549, .F. ) ;
#13745 = CARTESIAN_POINT ( 'NONE',  ( -2.651650429449552870, 3.125000000000000000, -0.8483495705504462414 ) ) ;
#13746 = APPROVAL_ROLE ( '' ) ;
#13747 = EDGE_CURVE ( 'NONE', #9221, #2235, #6203, .T. ) ;
#13748 = DIRECTION ( 'NONE',  ( 0.000000000000000000, -0.8087231630780308267, -0.5881894639493849830 ) ) ;
#13749 = FACE_OUTER_BOUND ( 'NONE', #10238, .T. ) ;
#13750 = ORIENTED_EDGE ( 'NONE', *, *, #8014, .F. ) ;
#13751 = CARTESIAN_POINT ( 'NONE',  ( 26.15341798802279527, 6.000000000000000000, -138.2600702976168350 ) ) ;
#13752 = CARTESIAN_POINT ( 'NONE',  ( 2.298097038856278029, 5.125000000000000000, -5.798097038856279362 ) ) ;
#13753 = DIRECTION ( 'NONE',  ( -8.764770998266003672E-18, 0.000000000000000000, -1.000000000000000000 ) ) ;
#13754 = CARTESIAN_POINT ( 'NONE',  ( -10.71664336931383588, 2.500000000000000444, -125.5340273011801884 ) ) ;
#13755 = CARTESIAN_POINT ( 'NONE',  ( -1.553300858899106629, 8.562500000000001776, 0.2499999999999998335 ) ) ;
#13756 = CARTESIAN_POINT ( 'NONE',  ( 1.553300858899108849, 12.93750000000000355, 0.2499999999999993616 ) ) ;
#13757 = DIRECTION ( 'NONE',  ( 0.000000000000000000, 0.000000000000000000, -1.000000000000000000 ) ) ;
#13758 = VERTEX_POINT ( 'NONE', #14596 ) ;
#13759 = CARTESIAN_POINT ( 'NONE',  ( -9.108720832937448719, 2.673239310146674708, -116.5073105006876375 ) ) ;
#13760 = CARTESIAN_POINT ( 'NONE',  ( -3.750000000000000000, 9.687500000000000000, -1.946699141100893149 ) ) ;
#13761 = CARTESIAN_POINT ( 'NONE',  ( 4.675654263134669364, 1.363187254327671670E-15, -31.10957739081536033 ) ) ;
#13762 = CARTESIAN_POINT ( 'NONE',  ( 27.95136620086945456, 7.321094445766561876, -28.22695831649836151 ) ) ;
#13763 = EDGE_CURVE ( 'NONE', #4341, #2589, #13376, .T. ) ;
#13764 = DIRECTION ( 'NONE',  ( -0.000000000000000000, 1.000000000000000000, -0.000000000000000000 ) ) ;
#13765 = ORIENTED_EDGE ( 'NONE', *, *, #5789, .F. ) ;
#13766 = CARTESIAN_POINT ( 'NONE',  ( -27.92420520952412488, -2.185846814899320366E-12, -179.9270560460287811 ) ) ;
#13767 = CARTESIAN_POINT ( 'NONE',  ( 9.922656535062992944, 0.1207761337397980084, -163.9774224701945968 ) ) ;
#13768 = CARTESIAN_POINT ( 'NONE',  ( -50.19288965972938854, 9.999999999999998224, -165.3052356888205168 ) ) ;
#13769 = CARTESIAN_POINT ( 'NONE',  ( -3.980102097228897738E-16, 1.000000000000000000, -6.749999999999999112 ) ) ;
#13770 = VERTEX_POINT ( 'NONE', #5231 ) ;
#13771 = CARTESIAN_POINT ( 'NONE',  ( 1.831246893856133928, -2.490287375297125294, -1.000000000000000888 ) ) ;
#13772 = DIRECTION ( 'NONE',  ( 0.000000000000000000, 1.000000000000000000, 0.000000000000000000 ) ) ;
#13773 = CARTESIAN_POINT ( 'NONE',  ( -25.68027788593440874, 1.265875433067397582, -206.1712788784230099 ) ) ;
#13774 = CARTESIAN_POINT ( 'NONE',  ( -2.298097038856278473, 10.12500000000000000, -1.201902961143720416 ) ) ;
#13775 = CARTESIAN_POINT ( 'NONE',  ( 8.963175985653281330, 12.17508258105334917, 1.589461697835446774 ) ) ;
#13776 = CARTESIAN_POINT ( 'NONE',  ( 4.999999996894303855, 8.673617379884035472E-16, -101.5775160893583546 ) ) ;
#13777 = CARTESIAN_POINT ( 'NONE',  ( -1.346194077712558945, 7.562500000000000888, -0.2500000000000002220 ) ) ;
#13778 = CARTESIAN_POINT ( 'NONE',  ( -1.553300858899107073, -0.06249999999999988898, -7.249999999999999112 ) ) ;
#13779 = CARTESIAN_POINT ( 'NONE',  ( 0.000000000000000000, -0.2105996885190176415, -0.1347136637304948981 ) ) ;
#13780 = CARTESIAN_POINT ( 'NONE',  ( 1.397354133952893873, 2.559042896907057774, -1.000000000000001332 ) ) ;
#13781 = CARTESIAN_POINT ( 'NONE',  ( 2.298097038856279362, 12.87500000000000178, -1.201902961143720860 ) ) ;
#13782 = EDGE_CURVE ( 'NONE', #3650, #13806, #6449, .T. ) ;
#13783 = CARTESIAN_POINT ( 'NONE',  ( -8.484577415225384556, 9.999999999999996447, -105.8546082955197392 ) ) ;
#13784 = CARTESIAN_POINT ( 'NONE',  ( 4.728979099990255897, 14.51970457313589513, 1.390952412700756868 ) ) ;
#13785 = CARTESIAN_POINT ( 'NONE',  ( -3.249999999999999556, 9.250000000000000000, -3.499999999999999556 ) ) ;
#13786 = CARTESIAN_POINT ( 'NONE',  ( 4.349367571369147534, 0.000000000000000000, -126.8184404512878984 ) ) ;
#13787 = FACE_OUTER_BOUND ( 'NONE', #8788, .T. ) ;
#13788 = ORIENTED_EDGE ( 'NONE', *, *, #10729, .T. ) ;
#13789 = EDGE_LOOP ( 'NONE', ( #9564, #13097, #13944, #13738 ) ) ;
#13790 = CARTESIAN_POINT ( 'NONE',  ( 8.414431238570866611, 12.50000000000000000, -115.4905761430241142 ) ) ;
#13791 = CARTESIAN_POINT ( 'NONE',  ( -3.750000000000000000, 1.250000000000000000, -3.499999999999999112 ) ) ;
#13792 = CARTESIAN_POINT ( 'NONE',  ( -4.592425496802573972E-16, 2.000000000000000000, -7.250000000000000000 ) ) ;
#13793 = CARTESIAN_POINT ( 'NONE',  ( -3.980102097228897738E-16, 13.00000000000000000, -6.749999999999999112 ) ) ;
#13794 = VERTEX_POINT ( 'NONE', #12015 ) ;
#13795 = CARTESIAN_POINT ( 'NONE',  ( -3.249999999999999556, 10.25000000000000000, -3.499999999999999556 ) ) ;
#13796 = DIRECTION ( 'NONE',  ( 0.9961255586397054218, -0.000000000000000000, -0.08794243244722428632 ) ) ;
#13797 = CARTESIAN_POINT ( 'NONE',  ( -8.068063733882274491, 13.23099846074044095, -104.6727491793208600 ) ) ;
#13798 = SHAPE_REPRESENTATION_RELATIONSHIP ( 'NONE' , 'NONE' ,  #9812, #7414 ) ;
#13799 = CARTESIAN_POINT ( 'NONE',  ( -9.868623143903928252, 9.999999999999996447, -115.7530035192428528 ) ) ;
#13800 = PERSON_AND_ORGANIZATION_ROLE ( 'creator' ) ;
#13801 = CARTESIAN_POINT ( 'NONE',  ( 8.317394296398017417, 15.00000000000000000, -114.4625571486813556 ) ) ;
#13802 = CARTESIAN_POINT ( 'NONE',  ( 3.220286340258128543, 14.96835584425696730, -12.99882895025039531 ) ) ;
#13803 = EDGE_LOOP ( 'NONE', ( #3551, #5194, #3272, #10400 ) ) ;
#13804 = CARTESIAN_POINT ( 'NONE',  ( 21.56441208847391167, 7.880035444290784328E-10, -138.8172008007609008 ) ) ;
#13805 = CARTESIAN_POINT ( 'NONE',  ( -3.249999999999999556, 12.18750000000000000, -2.153805922287440833 ) ) ;
#13806 = VERTEX_POINT ( 'NONE', #13273 ) ;
#13807 = CARTESIAN_POINT ( 'NONE',  ( 1.346194077712558057, 5.562500000000000000, -6.750000000000000000 ) ) ;
#13808 = CARTESIAN_POINT ( 'NONE',  ( -1.528156170053301510, 7.379999999999995453, -45.73714083922575213 ) ) ;
#13809 = CARTESIAN_POINT ( 'NONE',  ( 1.553300858899105963, 1.062500000000000444, -7.250000000000000888 ) ) ;
#13810 = EDGE_LOOP ( 'NONE', ( #2201, #6191, #4988, #6109, #11609, #12658, #4929, #8773 ) ) ;
#13811 = LINE ( 'NONE', #6544, #1067 ) ;
#13812 = CARTESIAN_POINT ( 'NONE',  ( -3.980102097228897245E-16, 0.5000000000000000000, -6.749999999999999112 ) ) ;
#13813 = CARTESIAN_POINT ( 'NONE',  ( 3.749999999999998668, 5.687500000000000000, -5.053300858899107517 ) ) ;
#13814 = CARTESIAN_POINT ( 'NONE',  ( -25.29848011718828005, 1.467800717594119675, -207.1124310616453954 ) ) ;
#13815 = CARTESIAN_POINT ( 'NONE',  ( 0.2330829912941287385, 3.741858015452750319, 2.640135352774355404 ) ) ;
#13816 = CALENDAR_DATE ( 2026, 8, 10 ) ;
#13817 = CARTESIAN_POINT ( 'NONE',  ( 8.362033940405666499, 5.000000000000000888, -112.8158568780617941 ) ) ;
#13818 = DIRECTION ( 'NONE',  ( 0.9997619372588931741, 0.000000000000000000, 0.02181900108494707474 ) ) ;
#13819 = SECURITY_CLASSIFICATION ( '', '', #7857 ) ;
#13820 = ORIENTED_EDGE ( 'NONE', *, *, #8631, .T. ) ;
#13821 = CARTESIAN_POINT ( 'NONE',  ( 0.000000000000000000, 3.500000000000000000, -0.2500000000000002220 ) ) ;
#13822 = EDGE_CURVE ( 'NONE', #10395, #4505, #12094, .T. ) ;
#13823 = EDGE_CURVE ( 'NONE', #4833, #5493, #6231, .T. ) ;
#13824 = CARTESIAN_POINT ( 'NONE',  ( -17.32624372123753886, 2.500000000000000444, -122.3796757791585321 ) ) ;
#13825 = CARTESIAN_POINT ( 'NONE',  ( 2.651650429449552870, 10.12500000000000000, -6.151650429449553314 ) ) ;
#13826 = CARTESIAN_POINT ( 'NONE',  ( -2.651650429449553314, 13.37500000000000000, -6.151650429449552426 ) ) ;
#13827 = CC_DESIGN_SECURITY_CLASSIFICATION ( #4938, ( #15319 ) ) ;
#13828 = CARTESIAN_POINT ( 'NONE',  ( -65.80676792586451995, 14.98942443719950113, -191.1849550162216929 ) ) ;
#13829 = ORIENTED_EDGE ( 'NONE', *, *, #5371, .F. ) ;
#13830 = CARTESIAN_POINT ( 'NONE',  ( 22.05734493763781146, -2.051692149507289097E-14, 29.73364058993714565 ) ) ;
#13831 = CARTESIAN_POINT ( 'NONE',  ( 2.298097038856278029, 1.124999999999999778, -5.798097038856279362 ) ) ;
#13832 = CARTESIAN_POINT ( 'NONE',  ( 11.30303403385899941, 12.83532670273191556, -106.4054638337314458 ) ) ;
#13833 = AXIS2_PLACEMENT_3D ( 'NONE', #10838, #3815, #12942 ) ;
#13834 = ADVANCED_FACE ( 'NONE', ( #14519 ), #1322, .T. ) ;
#13835 = PERSON_AND_ORGANIZATION ( #3176, #3020 ) ;
#13836 = DIRECTION ( 'NONE',  ( 0.000000000000000000, -0.000000000000000000, 1.000000000000000000 ) ) ;
#13837 = ORIENTED_EDGE ( 'NONE', *, *, #14130, .F. ) ;
#13838 = CARTESIAN_POINT ( 'NONE',  ( -23.34801257951161091, 8.673617379884035472E-16, -203.6232164356695762 ) ) ;
#13839 = CARTESIAN_POINT ( 'NONE',  ( 0.000000000000000000, 0.000000000000000000, -0.2500000000000002220 ) ) ;
#13840 = CARTESIAN_POINT ( 'NONE',  ( -41.55509581777007355, 9.999999999999998224, -158.0567977603521115 ) ) ;
#13841 = VECTOR ( 'NONE', #402, 1000.000000000000000 ) ;
#13842 = CARTESIAN_POINT ( 'NONE',  ( -1.346194077712558945, 2.562500000000000444, -0.2500000000000002220 ) ) ;
#13843 = ORIENTED_EDGE ( 'NONE', *, *, #10056, .T. ) ;
#13844 = CARTESIAN_POINT ( 'NONE',  ( -7.699506734510488393, 15.00000000000000000, -129.6777018991784018 ) ) ;
#13845 = AXIS2_PLACEMENT_3D ( 'NONE', #9825, #9752, #14715 ) ;
#13846 = CARTESIAN_POINT ( 'NONE',  ( 4.286263797015736595E-16, 0.000000000000000000, 3.500000000000000000 ) ) ;
#13847 = AXIS2_PLACEMENT_3D ( 'NONE', #8061, #10604, #7048 ) ;
#13848 = CARTESIAN_POINT ( 'NONE',  ( -4.507463604512252253, 0.000000000000000000, -2.585105772303598393 ) ) ;
#13849 = AXIS2_PLACEMENT_3D ( 'NONE', #11041, #4246, #5166 ) ;
#13850 = DIRECTION ( 'NONE',  ( 0.000000000000000000, 0.000000000000000000, 1.000000000000000000 ) ) ;
#13851 = EDGE_CURVE ( 'NONE', #11832, #2518, #14622, .T. ) ;
#13852 = CARTESIAN_POINT ( 'NONE',  ( 3.559460973860744559, 8.673617379884035472E-16, -107.0011611385543233 ) ) ;
#13853 = CARTESIAN_POINT ( 'NONE',  ( 3.249999999999998224, 13.31250000000000178, -2.153805922287439945 ) ) ;
#13854 = CARTESIAN_POINT ( 'NONE',  ( -29.69515346086420138, 9.999999999999998224, -156.7390981038714983 ) ) ;
#13855 = CARTESIAN_POINT ( 'NONE',  ( 3.750000000000000000, 3.312500000000000000, -1.946699141100892705 ) ) ;
#13856 = FACE_OUTER_BOUND ( 'NONE', #2364, .T. ) ;
#13857 = CIRCLE ( 'NONE', #7433, 0.4999999999999995559 ) ;
#13858 = CARTESIAN_POINT ( 'NONE',  ( -4.090890948359609425, 15.00000000000000000, -103.1929727064838289 ) ) ;
#13859 = CARTESIAN_POINT ( 'NONE',  ( -1.346194077712559389, 14.06249999999999822, -0.2500000000000002220 ) ) ;
#13860 = CARTESIAN_POINT ( 'NONE',  ( -5.507086477070941122, 10.00000000000000178, -116.3025817345989168 ) ) ;
#13861 = CARTESIAN_POINT ( 'NONE',  ( 4.856804767890306351, 14.90536770052033866, -1.840041787218210878 ) ) ;
#13862 = CARTESIAN_POINT ( 'NONE',  ( 3.249999999999999556, 9.750000000000000000, -3.500000000000000000 ) ) ;
#13863 = DIRECTION ( 'NONE',  ( 0.000000000000000000, 0.000000000000000000, 1.000000000000000000 ) ) ;
#13864 = CARTESIAN_POINT ( 'NONE',  ( 2.449293598294706414E-16, 4.000000000000000000, 2.000000000000000000 ) ) ;
#13865 = ORIENTED_EDGE ( 'NONE', *, *, #1113, .T. ) ;
#13866 = ORIENTED_EDGE ( 'NONE', *, *, #1400, .T. ) ;
#13867 = CARTESIAN_POINT ( 'NONE',  ( 13.05859050630842333, 12.50000000000000000, -125.1312933577355437 ) ) ;
#13868 = CARTESIAN_POINT ( 'NONE',  ( -2.651650429449553314, 2.375000000000000000, -6.151650429449552426 ) ) ;
#13869 = CARTESIAN_POINT ( 'NONE',  ( -1.346194077712559167, 14.93750000000000000, -6.749999999999999112 ) ) ;
#13870 = CARTESIAN_POINT ( 'NONE',  ( -7.218906882868092012, 2.500000000000000444, -107.2047439207351829 ) ) ;
#13871 = ORIENTED_EDGE ( 'NONE', *, *, #164, .T. ) ;
#13872 = AXIS2_PLACEMENT_3D ( 'NONE', #14752, #5304, #5230 ) ;
#13873 = EDGE_CURVE ( 'NONE', #14924, #10654, #14360, .T. ) ;
#13874 = CARTESIAN_POINT ( 'NONE',  ( -1.346194077712558945, 0.5625000000000001110, -0.2500000000000002220 ) ) ;
#13875 = EDGE_CURVE ( 'NONE', #1578, #9311, #12403, .T. ) ;
#13876 = EDGE_CURVE ( 'NONE', #4807, #2207, #2911, .T. ) ;
#13877 = CARTESIAN_POINT ( 'NONE',  ( -3.485185982199345389, -2.570071824251316084, -1.000000000000001332 ) ) ;
#13878 = DIRECTION ( 'NONE',  ( 0.000000000000000000, 0.000000000000000000, -1.000000000000000000 ) ) ;
#13879 =( NAMED_UNIT ( * ) PLANE_ANGLE_UNIT ( ) SI_UNIT ( $, .RADIAN. ) );
#13880 = CC_DESIGN_PERSON_AND_ORGANIZATION_ASSIGNMENT ( #6433, #490, ( #10001 ) ) ;
#13881 = CARTESIAN_POINT ( 'NONE',  ( -3.249999999999999556, 3.187500000000000000, -2.153805922287440833 ) ) ;
#13882 = APPROVAL_STATUS ( 'not_yet_approved' ) ;
#13883 = CC_DESIGN_APPROVAL ( #2249, ( #10001 ) ) ;
#13884 = CARTESIAN_POINT ( 'NONE',  ( 11.05697737879504494, 12.49999999999999822, -122.2826711085474756 ) ) ;
#13885 = CARTESIAN_POINT ( 'NONE',  ( -4.580007248818704468, 15.00000000000000533, -117.4298695725142920 ) ) ;
#13886 = ORIENTED_EDGE ( 'NONE', *, *, #12150, .T. ) ;
#13887 = CARTESIAN_POINT ( 'NONE',  ( 21.54700699050549773, -3.203769437592921893E-16, -138.7416251624139818 ) ) ;
#13888 = CARTESIAN_POINT ( 'NONE',  ( 3.249999999999998668, 9.687500000000000000, -4.846194077712560500 ) ) ;
#13889 = ORIENTED_EDGE ( 'NONE', *, *, #2712, .F. ) ;
#13890 = ORIENTED_EDGE ( 'NONE', *, *, #12128, .T. ) ;
#13891 = CARTESIAN_POINT ( 'NONE',  ( 2.298097038856278473, 2.625000000000000000, -5.798097038856279362 ) ) ;
#13892 = CARTESIAN_POINT ( 'NONE',  ( -9.629162051845682413, 4.000000000000000888, -147.9061454275191636 ) ) ;
#13893 = CARTESIAN_POINT ( 'NONE',  ( -3.750000000000000000, 2.687500000000000888, -1.946699141100893149 ) ) ;
#13894 = CARTESIAN_POINT ( 'NONE',  ( 1.346194077712561166, 6.437500000000000888, -0.2500000000000011102 ) ) ;
#13895 = VERTEX_POINT ( 'NONE', #4370 ) ;
#13896 = DIRECTION ( 'NONE',  ( 0.000000000000000000, -1.000000000000000000, 0.000000000000000000 ) ) ;
#13897 = CARTESIAN_POINT ( 'NONE',  ( -0.01496453197141594735, 5.000000000000000000, -5.196130874293185542 ) ) ;
#13898 = SECURITY_CLASSIFICATION ( '', '', #2691 ) ;
#13899 = CC_DESIGN_DATE_AND_TIME_ASSIGNMENT ( #3445, #12964, ( #10487 ) ) ;
#13900 = CARTESIAN_POINT ( 'NONE',  ( 2.298097038856278473, 11.62500000000000000, -5.798097038856279362 ) ) ;
#13901 = CARTESIAN_POINT ( 'NONE',  ( -2.651650429449553314, 4.375000000000000000, -6.151650429449552426 ) ) ;
#13902 = CARTESIAN_POINT ( 'NONE',  ( -25.28590446626877863, 0.04176024460088630791, -200.8353957342116587 ) ) ;
#13903 = DIRECTION ( 'NONE',  ( -0.000000000000000000, -1.000000000000000000, -0.000000000000000000 ) ) ;
#13904 = AXIS2_PLACEMENT_3D ( 'NONE', #12455, #11289, #7657 ) ;
#13905 = PERSON_AND_ORGANIZATION ( #3176, #3020 ) ;
#13906 = CARTESIAN_POINT ( 'NONE',  ( 8.644432307942668814, 5.000000000000001776, -116.7877792220761961 ) ) ;
#13907 = CARTESIAN_POINT ( 'NONE',  ( 8.895558325401111688, 6.000000000000000000, -125.4560052468458906 ) ) ;
#13908 = ORIENTED_EDGE ( 'NONE', *, *, #10366, .F. ) ;
#13909 = CARTESIAN_POINT ( 'NONE',  ( -3.249999999999999112, 5.687500000000000888, -2.153805922287440833 ) ) ;
#13910 = CARTESIAN_POINT ( 'NONE',  ( 9.103295372165979060, 15.00000000000043165, -106.0245955897191124 ) ) ;
#13911 = AXIS2_PLACEMENT_3D ( 'NONE', #4160, #7383, #12105 ) ;
#13912 = CARTESIAN_POINT ( 'NONE',  ( -3.750000000000000000, 7.812500000000000000, -5.053300858899105741 ) ) ;
#13913 = CARTESIAN_POINT ( 'NONE',  ( 3.750000000000000000, 14.75000000000000178, -3.500000000000000444 ) ) ;
#13914 = CARTESIAN_POINT ( 'NONE',  ( -64.36898479267240702, 13.53642980808444563, -200.3260915304600189 ) ) ;
#13915 = ORIENTED_EDGE ( 'NONE', *, *, #517, .T. ) ;
#13916 = DIRECTION ( 'NONE',  ( -0.9997619372588931741, -0.000000000000000000, -0.02181900108494707821 ) ) ;
#13917 = CARTESIAN_POINT ( 'NONE',  ( -3.750000000000000000, 12.68750000000000000, -1.946699141100893149 ) ) ;
#13918 = DIRECTION ( 'NONE',  ( 0.000000000000000000, -1.000000000000000000, 0.000000000000000000 ) ) ;
#13919 =( LENGTH_UNIT ( ) NAMED_UNIT ( * ) SI_UNIT ( .MILLI., .METRE. ) );
#13920 = CARTESIAN_POINT ( 'NONE',  ( -3.284464116416026425, 9.999999999999996447, -42.88872331408225591 ) ) ;
#13921 = ORIENTED_EDGE ( 'NONE', *, *, #3173, .T. ) ;
#13922 = DIRECTION ( 'NONE',  ( 0.000000000000000000, -0.000000000000000000, 1.000000000000000000 ) ) ;
#13923 = CARTESIAN_POINT ( 'NONE',  ( 11.11125876792575085, 0.7539515673351797620, -165.0738428850340540 ) ) ;
#13924 = CARTESIAN_POINT ( 'NONE',  ( -58.73854075876246128, 9.999999999999998224, -181.3184243508228519 ) ) ;
#13925 = CARTESIAN_POINT ( 'NONE',  ( 1.346194077712558279, 1.062500000000000444, -6.750000000000000888 ) ) ;
#13926 = ORIENTED_EDGE ( 'NONE', *, *, #10937, .F. ) ;
#13927 = DIRECTION ( 'NONE',  ( -0.000000000000000000, -1.000000000000000000, 0.000000000000000000 ) ) ;
#13928 = LINE ( 'NONE', #11669, #1836 ) ;
#13929 = CARTESIAN_POINT ( 'NONE',  ( 8.935548306746156300, 9.999999999999880984, 2.855381328098128613 ) ) ;
#13930 = CARTESIAN_POINT ( 'NONE',  ( -0.3675725891509502574, 0.000000000000000000, -0.3389548520155299949 ) ) ;
#13931 = VECTOR ( 'NONE', #840, 1000.000000000000114 ) ;
#13932 = CARTESIAN_POINT ( 'NONE',  ( 3.249999999999998224, 12.31250000000000178, -2.153805922287439945 ) ) ;
#13933 = CARTESIAN_POINT ( 'NONE',  ( 2.449293598294706414E-16, 4.000000000000000000, 2.000000000000000000 ) ) ;
#13934 = CARTESIAN_POINT ( 'NONE',  ( -3.750000000000000000, 2.687500000000000888, -1.946699141100893149 ) ) ;
#13935 = CARTESIAN_POINT ( 'NONE',  ( 0.000000000000000000, 0.000000000000000000, -0.2500000000000002220 ) ) ;
#13936 = CARTESIAN_POINT ( 'NONE',  ( 6.369258321017759350, -2.075239479414269894, -34.56909192082981974 ) ) ;
#13937 = CARTESIAN_POINT ( 'NONE',  ( -7.250352174397651339, 10.00000000000000355, -120.6338660983546589 ) ) ;
#13938 = ADVANCED_FACE ( 'NONE', ( #7915 ), #4236, .T. ) ;
#13939 = CARTESIAN_POINT ( 'NONE',  ( 4.075001113472075609, 13.47049942401578448, 3.499674426787218184 ) ) ;
#13940 = CARTESIAN_POINT ( 'NONE',  ( 1.346194077712558057, 9.562500000000000000, -6.750000000000000000 ) ) ;
#13941 = AXIS2_PLACEMENT_3D ( 'NONE', #1186, #2423, #5889 ) ;
#13942 = CARTESIAN_POINT ( 'NONE',  ( -9.240119717576689595, 9.999999999999998224, -104.6630069175297564 ) ) ;
#13943 = CARTESIAN_POINT ( 'NONE',  ( 4.053227644665166274, 5.000000000000000000, -106.4152912718141266 ) ) ;
#13944 = ORIENTED_EDGE ( 'NONE', *, *, #1841, .F. ) ;
#13945 = VERTEX_POINT ( 'NONE', #796 ) ;
#13946 = CARTESIAN_POINT ( 'NONE',  ( 8.701636889681944709, 12.50000000000000355, -110.9796434783077359 ) ) ;
#13947 = CARTESIAN_POINT ( 'NONE',  ( 0.000000000000000000, 5.000000000000000000, 0.2500000000000002220 ) ) ;
#13948 = CARTESIAN_POINT ( 'NONE',  ( 1.553300858899109071, 1.437500000000000000, 0.2499999999999989175 ) ) ;
#13949 = DIRECTION ( 'NONE',  ( 0.000000000000000000, 0.000000000000000000, -1.000000000000000000 ) ) ;
#13950 = ORIENTED_EDGE ( 'NONE', *, *, #14056, .T. ) ;
#13951 = CARTESIAN_POINT ( 'NONE',  ( 2.298097038856278029, 2.125000000000000000, -5.798097038856279362 ) ) ;
#13952 = PRODUCT_RELATED_PRODUCT_CATEGORY ( 'detail', '', ( #14121 ) ) ;
#13953 = CARTESIAN_POINT ( 'NONE',  ( -53.51085313097401297, 15.00000000000000000, -156.4046016528996859 ) ) ;
#13954 = CARTESIAN_POINT ( 'NONE',  ( 51.62524086895222553, 0.000000000000000000, 69.88209797381236399 ) ) ;
#13955 = SHAPE_REPRESENTATION_RELATIONSHIP ( 'NONE' , 'NONE' ,  #12380, #10006 ) ;
#13956 = CARTESIAN_POINT ( 'NONE',  ( 2.298097038856279362, 5.875000000000000000, -1.201902961143720860 ) ) ;
#13957 = APPROVAL_DATE_TIME ( #12946, #548 ) ;
#13958 = EDGE_CURVE ( 'NONE', #14484, #11635, #6585, .T. ) ;
#13959 = CARTESIAN_POINT ( 'NONE',  ( 9.781725384838754422, 12.49999999999999822, -108.7377634488177165 ) ) ;
#13960 = CARTESIAN_POINT ( 'NONE',  ( 1.855481649321436777, 15.00000000000000000, -35.83830032691820122 ) ) ;
#13961 = ORIENTED_EDGE ( 'NONE', *, *, #10461, .F. ) ;
#13962 = ADVANCED_FACE ( 'NONE', ( #14877 ), #12871, .T. ) ;
#13963 = CARTESIAN_POINT ( 'NONE',  ( -24.86990227130816322, 15.00000000000000000, -145.8847246090277281 ) ) ;
#13964 = CARTESIAN_POINT ( 'NONE',  ( 3.249999999999998668, 12.68750000000000178, -4.846194077712560500 ) ) ;
#13965 = ORIENTED_EDGE ( 'NONE', *, *, #14661, .T. ) ;
#13966 = ORIENTED_EDGE ( 'NONE', *, *, #11673, .T. ) ;
#13967 = CARTESIAN_POINT ( 'NONE',  ( -3.750000000000000000, 11.81250000000000178, -5.053300858899105741 ) ) ;
#13968 = CARTESIAN_POINT ( 'NONE',  ( -3.724891368794482904, 9.650666666666662508, -47.87745094654707145 ) ) ;
#13969 = CARTESIAN_POINT ( 'NONE',  ( 2.651650429449554203, 1.375000000000000000, -0.8483495705504471296 ) ) ;
#13970 = CARTESIAN_POINT ( 'NONE',  ( -1.346194077712558945, 7.562500000000000888, -0.2500000000000002220 ) ) ;
#13971 = ORIENTED_EDGE ( 'NONE', *, *, #9151, .F. ) ;
#13972 = CARTESIAN_POINT ( 'NONE',  ( -5.836146573691745942, 14.76824404323223128, -116.8702851668251839 ) ) ;
#13973 = CARTESIAN_POINT ( 'NONE',  ( 2.298097038856279362, 4.875000000000000000, -1.201902961143720860 ) ) ;
#13974 = CARTESIAN_POINT ( 'NONE',  ( 3.750000000000000000, 4.750000000000000000, -3.500000000000000444 ) ) ;
#13975 = CARTESIAN_POINT ( 'NONE',  ( -25.42189670022433035, 0.8929212780356239332, -205.7249994877904840 ) ) ;
#13976 = FACE_OUTER_BOUND ( 'NONE', #10482, .T. ) ;
#13977 =( BOUNDED_SURFACE ( )  B_SPLINE_SURFACE ( 3, 3, ( 
 ( #8313, #12970, #8469, #3766, #4766, #2607, #1207 ),
 ( #1066, #7144, #7072, #9554, #8241, #14133, #5774 ),
 ( #14279, #12894, #3609, #1141, #15299, #3679, #5844 ),
 ( #11792, #4691, #9408, #8389, #14053, #5915, #3531 ) ),
 .UNSPECIFIED., .F., .F., .F. ) 
 B_SPLINE_SURFACE_WITH_KNOTS ( ( 4, 4 ),
 ( 4, 3, 4 ),
 ( 0.000000000000000000, 1.000000000000000000 ),
 ( 0.000000000000000000, 0.5000000000000000000, 1.000000000000000000 ),
 .UNSPECIFIED. ) 
 GEOMETRIC_REPRESENTATION_ITEM ( )  RATIONAL_B_SPLINE_SURFACE ( (
 ( 1.000000000000000000, 0.7662986988867873661, 0.7662986988867873661, 1.000000000000000000, 0.7662986988867873661, 0.7662986988867873661, 1.000000000000000000),
 ( 0.9216682375510407699, 0.7062731712406410400, 0.7062731712406410400, 0.9216682375510407699, 0.7062731712406410400, 0.7062731712406410400, 0.9216682375510407699),
 ( 0.9216682375510407699, 0.7062731712406410400, 0.7062731712406410400, 0.9216682375510407699, 0.7062731712406410400, 0.7062731712406410400, 0.9216682375510407699),
 ( 1.000000000000000000, 0.7662986988867873661, 0.7662986988867873661, 1.000000000000000000, 0.7662986988867873661, 0.7662986988867873661, 1.000000000000000000) ) ) 
 REPRESENTATION_ITEM ( '' )  SURFACE ( )  );
#13978 = PERSON_AND_ORGANIZATION_ROLE ( 'creator' ) ;
#13979 = CARTESIAN_POINT ( 'NONE',  ( 8.379952990905023213, 5.000000000000001776, -115.2049983755456282 ) ) ;
#13980 = EDGE_CURVE ( 'NONE', #12909, #8581, #11628, .T. ) ;
#13981 = EDGE_LOOP ( 'NONE', ( #735, #7920, #35, #8071 ) ) ;
#13982 = CARTESIAN_POINT ( 'NONE',  ( -1.346194077712558945, 6.562500000000000888, -0.2500000000000002220 ) ) ;
#13983 = CARTESIAN_POINT ( 'NONE',  ( 30.32986759126112730, 0.7500000000000000000, 43.04214087805580391 ) ) ;
#13984 = CARTESIAN_POINT ( 'NONE',  ( 2.651650429449552870, 8.125000000000000000, -6.151650429449553314 ) ) ;
#13985 = CARTESIAN_POINT ( 'NONE',  ( -3.750000000000000000, 13.25000000000000000, -3.499999999999999112 ) ) ;
#13986 = FACE_OUTER_BOUND ( 'NONE', #3324, .T. ) ;
#13987 = CARTESIAN_POINT ( 'NONE',  ( 0.000000000000000000, 9.999999999999998224, -100.6237003951525679 ) ) ;
#13988 = CARTESIAN_POINT ( 'NONE',  ( 0.000000000000000000, 12.50000000000000178, 0.2500000000000002220 ) ) ;
#13989 = CARTESIAN_POINT ( 'NONE',  ( -4.873992731081242091, 4.336808689942016750E-16, -121.4575503408599957 ) ) ;
#13990 = SECURITY_CLASSIFICATION_LEVEL ( 'unclassified' ) ;
#13991 = PRODUCT_DEFINITION_SHAPE ( 'NONE', 'NONE',  #15321 ) ;
#13992 = CARTESIAN_POINT ( 'NONE',  ( 11.32016196459912649, 5.000000000000000888, -106.4092894470390291 ) ) ;
#13993 = VERTEX_POINT ( 'NONE', #7663 ) ;
#13994 = CARTESIAN_POINT ( 'NONE',  ( 5.845480107720362639, 3.062150895296549269, 4.850269518005670299 ) ) ;
#13995 = CARTESIAN_POINT ( 'NONE',  ( -3.249999999999999556, 4.312500000000000888, -4.846194077712557835 ) ) ;
#13996 = CARTESIAN_POINT ( 'NONE',  ( -61.70104298247990471, 9.999999999999998224, -192.5140885290205119 ) ) ;
#13997 = CARTESIAN_POINT ( 'NONE',  ( 2.298097038856278029, 3.125000000000000444, -5.798097038856279362 ) ) ;
#13998 = ORIENTED_EDGE ( 'NONE', *, *, #14130, .T. ) ;
#13999 = DIRECTION ( 'NONE',  ( 0.000000000000000000, 0.000000000000000000, 1.000000000000000000 ) ) ;
#14000 = CARTESIAN_POINT ( 'NONE',  ( 29.21736815051483660, 8.773889247172311556, -44.21329492081407153 ) ) ;
#14001 = CIRCLE ( 'NONE', #5356, 1.101020514433642683 ) ;
#14002 = FACE_OUTER_BOUND ( 'NONE', #5874, .T. ) ;
#14003 = CARTESIAN_POINT ( 'NONE',  ( 0.7716514365823460286, 1.734723475976807094E-15, -111.8714012163897280 ) ) ;
#14004 = CARTESIAN_POINT ( 'NONE',  ( 1.346194077712558279, 11.06250000000000178, -6.750000000000000888 ) ) ;
#14005 = CARTESIAN_POINT ( 'NONE',  ( 6.491365067585770809, 12.49999999999999822, 0.2705411889128697123 ) ) ;
#14006 = CARTESIAN_POINT ( 'NONE',  ( -3.750000000000000000, 1.687500000000000222, -1.946699141100893149 ) ) ;
#14007 = CARTESIAN_POINT ( 'NONE',  ( -4.878500514246746356, 4.999999999999999112, -144.3544516087390264 ) ) ;
#14008 = CARTESIAN_POINT ( 'NONE',  ( -8.445519633954337024, 12.12030021904079113, -105.2770060228727118 ) ) ;
#14009 = VECTOR ( 'NONE', #14740, 1000.000000000000000 ) ;
#14010 = DIRECTION ( 'NONE',  ( 0.000000000000000000, 1.000000000000000000, 0.000000000000000000 ) ) ;
#14011 = CARTESIAN_POINT ( 'NONE',  ( -0.4094286939087771193, 2.100000000000851408, 42.04785295243777199 ) ) ;
#14012 = CARTESIAN_POINT ( 'NONE',  ( 2.298097038856278473, 13.62500000000000000, -5.798097038856279362 ) ) ;
#14013 = CARTESIAN_POINT ( 'NONE',  ( 20.38723710659885313, 5.321094445766561876, -31.17704722822712426 ) ) ;
#14014 = CARTESIAN_POINT ( 'NONE',  ( 7.359540121889097897, 5.000000000000000888, -111.8458898531363275 ) ) ;
#14015 = VERTEX_POINT ( 'NONE', #2025 ) ;
#14016 = VERTEX_POINT ( 'NONE', #12687 ) ;
#14017 = DIRECTION ( 'NONE',  ( -1.000000000000000000, -0.000000000000000000, -0.000000000000000000 ) ) ;
#14018 = CARTESIAN_POINT ( 'NONE',  ( -3.750000000000000000, 3.250000000000000444, -3.499999999999999112 ) ) ;
#14019 = CARTESIAN_POINT ( 'NONE',  ( -3.749999999999999556, 2.750000000000000444, -3.499999999999999112 ) ) ;
#14020 = CARTESIAN_POINT ( 'NONE',  ( 8.595858757291594543, 9.999999999999998224, -113.5677547687719624 ) ) ;
#14021 = ORIENTED_EDGE ( 'NONE', *, *, #733, .F. ) ;
#14022 = CARTESIAN_POINT ( 'NONE',  ( -3.980102097228897738E-16, 2.000000000000000000, -6.749999999999999112 ) ) ;
#14023 = ADVANCED_FACE ( 'NONE', ( #9203 ), #13708, .F. ) ;
#14024 = CARTESIAN_POINT ( 'NONE',  ( -8.749806588114527273, 15.00000000000000000, -116.1271478199639944 ) ) ;
#14025 = CARTESIAN_POINT ( 'NONE',  ( 5.844703153020811115, 5.000000000000000888, -103.2023327213425432 ) ) ;
#14026 = CARTESIAN_POINT ( 'NONE',  ( 1.346194077712558057, 4.562500000000000888, -6.750000000000000000 ) ) ;
#14027 = CALENDAR_DATE ( 2026, 8, 10 ) ;
#14028 = B_SPLINE_CURVE_WITH_KNOTS ( 'NONE', 3,
 ( #13678, #3078, #1688, #6632, #11340, #4097, #5149, #6145, #14674, #10783, #6308, #12178, #200, #11092, #8539, #7220, #11940, #3998, #4910, #4996, #1518, #13511, #2678, #2760, #9625, #3918, #6066, #363 ),
 .UNSPECIFIED., .F., .F.,
 ( 4, 2, 2, 2, 2, 2, 2, 2, 2, 2, 2, 2, 2, 4 ),
 ( 2.081668171172168513E-17, 0.006221094506044410298, 0.007776368132555515691, 0.009331641759066621952, 0.01244218901208886917, 0.01555273626511111638, 0.01866328351813336187, 0.02177383077115560908, 0.02488437802417785977, 0.03110547253022235420, 0.03421601978324460835, 0.03732656703626685557, 0.04354766154231135000, 0.04976875604835584443 ),
 .UNSPECIFIED. ) ;
#14029 = DIRECTION ( 'NONE',  ( 0.000000000000000000, 1.000000000000000000, 0.000000000000000000 ) ) ;
#14030 = DIRECTION ( 'NONE',  ( 1.000000000000000000, 0.000000000000000000, 0.000000000000000000 ) ) ;
#14031 = ORIENTED_EDGE ( 'NONE', *, *, #5368, .T. ) ;
#14032 = DIRECTION ( 'NONE',  ( -0.02181900108494707127, 0.000000000000000000, 0.9997619372588931741 ) ) ;
#14033 = CARTESIAN_POINT ( 'NONE',  ( 3.249999999999998668, 10.68750000000000000, -4.846194077712560500 ) ) ;
#14034 = VERTEX_POINT ( 'NONE', #10361 ) ;
#14035 = EDGE_LOOP ( 'NONE', ( #2495, #15050, #4247, #9237 ) ) ;
#14036 = CARTESIAN_POINT ( 'NONE',  ( 2.651650429449552870, 10.12500000000000000, -6.151650429449555091 ) ) ;
#14037 = CARTESIAN_POINT ( 'NONE',  ( -3.665378489062163236, 2.331468351712828833E-16, 4.733462801983808532 ) ) ;
#14038 = CARTESIAN_POINT ( 'NONE',  ( -2.651650429449552870, 7.625000000000001776, -0.8483495705504463524 ) ) ;
#14039 = CARTESIAN_POINT ( 'NONE',  ( -2.298097038856278029, 6.625000000000000888, -1.201902961143720638 ) ) ;
#14040 = ORIENTED_EDGE ( 'NONE', *, *, #12124, .T. ) ;
#14041 = CARTESIAN_POINT ( 'NONE',  ( 6.276419674667793380, 14.49781573971641890, 2.481921665638175956 ) ) ;
#14042 = CARTESIAN_POINT ( 'NONE',  ( 2.298097038856278473, 3.625000000000000000, -5.798097038856279362 ) ) ;
#14043 = EDGE_CURVE ( 'NONE', #6374, #6272, #12345, .T. ) ;
#14044 = CARTESIAN_POINT ( 'NONE',  ( -1.553300858899106629, 5.062500000000001776, 0.2500000000000002220 ) ) ;
#14045 = EDGE_CURVE ( 'NONE', #7043, #14756, #4967, .T. ) ;
#14046 = CARTESIAN_POINT ( 'NONE',  ( -25.02010205735157555, 1.581731481081007251, -206.7284262751177550 ) ) ;
#14047 = LINE ( 'NONE', #10558, #14856 ) ;
#14048 = APPROVAL_DATE_TIME ( #12809, #4078 ) ;
#14049 = CARTESIAN_POINT ( 'NONE',  ( 1.831246893856137481, 2.490287375297123074, -1.000000000000007772 ) ) ;
#14050 = CARTESIAN_POINT ( 'NONE',  ( 30.32986759126112730, 0.7500000000000000000, 43.04214087805580391 ) ) ;
#14051 = VERTEX_POINT ( 'NONE', #7964 ) ;
#14052 = CARTESIAN_POINT ( 'NONE',  ( -3.249999999999999112, 8.812500000000001776, -4.846194077712558723 ) ) ;
#14053 = CARTESIAN_POINT ( 'NONE',  ( -6.119281984250456219, 2.490287375297125294, -44.38286699775952826 ) ) ;
#14054 = EDGE_CURVE ( 'NONE', #13993, #10578, #6057, .T. ) ;
#14055 = CARTESIAN_POINT ( 'NONE',  ( -3.750000000000000000, 8.687500000000003553, -1.946699141100893149 ) ) ;
#14056 = EDGE_CURVE ( 'NONE', #11802, #11095, #10288, .T. ) ;
#14057 = CARTESIAN_POINT ( 'NONE',  ( -3.750000000000000000, 13.31250000000000000, -5.053300858899105741 ) ) ;
#14058 = ADVANCED_FACE ( 'NONE', ( #11524 ), #11134, .T. ) ;
#14059 = CARTESIAN_POINT ( 'NONE',  ( -64.16515357636237127, 13.23091809669857888, -201.0642910017739950 ) ) ;
#14060 = CARTESIAN_POINT ( 'NONE',  ( -9.721966606378851239, 5.000000000000000888, -116.3614657639809309 ) ) ;
#14061 = CARTESIAN_POINT ( 'NONE',  ( 3.249999999999999556, 0.2500000000000001110, -3.500000000000000000 ) ) ;
#14062 = CARTESIAN_POINT ( 'NONE',  ( -5.449692324012782585, 4.336808689942018722E-16, -122.4844380376194835 ) ) ;
#14063 = COORDINATED_UNIVERSAL_TIME_OFFSET ( 0, 0, .AHEAD. ) ;
#14064 = DIRECTION ( 'NONE',  ( -0.000000000000000000, 1.000000000000000000, -0.000000000000000000 ) ) ;
#14065 = VERTEX_POINT ( 'NONE', #14801 ) ;
#14066 = DIRECTION ( 'NONE',  ( 0.6527336816407247611, 0.000000000000000000, -0.7575874476598360996 ) ) ;
#14067 = CARTESIAN_POINT ( 'NONE',  ( 3.249999999999999556, 1.750000000000000000, -3.500000000000000000 ) ) ;
#14068 = CARTESIAN_POINT ( 'NONE',  ( -52.59034431208613114, 15.00000000000000000, -168.6389827469745910 ) ) ;
#14069 = CARTESIAN_POINT ( 'NONE',  ( -2.298097038856279362, 4.875000000000000000, -5.798097038856278473 ) ) ;
#14070 = ORIENTED_EDGE ( 'NONE', *, *, #7047, .T. ) ;
#14071 = CARTESIAN_POINT ( 'NONE',  ( -6.178332509695485086, 9.999999999999998224, -118.3334666058101448 ) ) ;
#14072 = CARTESIAN_POINT ( 'NONE',  ( 4.507463604512255806, 5.000000000000000000, 2.585105772303601945 ) ) ;
#14073 = APPROVAL_PERSON_ORGANIZATION ( #7691, #10179, #14976 ) ;
#14074 = CARTESIAN_POINT ( 'NONE',  ( 6.183275261587990457, 13.32019864978253310, 4.031137569194784831 ) ) ;
#14075 = FACE_OUTER_BOUND ( 'NONE', #4583, .T. ) ;
#14076 = CARTESIAN_POINT ( 'NONE',  ( 1.346194077712558279, 12.06250000000000000, -6.750000000000000888 ) ) ;
#14077 = VECTOR ( 'NONE', #5731, 1000.000000000000000 ) ;
#14078 = CARTESIAN_POINT ( 'NONE',  ( 1.299830696487494386, 4.000000000000000000, -139.3994634862947635 ) ) ;
#14079 = CARTESIAN_POINT ( 'NONE',  ( 3.749999999999999556, 3.250000000000000000, -3.500000000000000444 ) ) ;
#14080 = CARTESIAN_POINT ( 'NONE',  ( -47.48189921986828210, 9.999999999999998224, -141.5723758807981483 ) ) ;
#14081 = LINE ( 'NONE', #10816, #3994 ) ;
#14082 = CARTESIAN_POINT ( 'NONE',  ( 26.71007981443200308, 4.628737540243305304, -136.8791680534709769 ) ) ;
#14083 = LOCAL_TIME ( 12, 28, 20.00000000000000000, #7443 ) ;
#14084 = CARTESIAN_POINT ( 'NONE',  ( -3.133172996766207419, 2.100000000000000089, 0.6152778258340406703 ) ) ;
#14085 = CARTESIAN_POINT ( 'NONE',  ( 1.346194077712558057, 14.56250000000000000, -6.750000000000000000 ) ) ;
#14086 = CIRCLE ( 'NONE', #11363, 3.187847681061608540 ) ;
#14087 = CIRCLE ( 'NONE', #9632, 3.500000000000000000 ) ;
#14088 = CARTESIAN_POINT ( 'NONE',  ( -8.678274320079829351, 12.27452600300057028, -104.4870831087946783 ) ) ;
#14089 = DIRECTION ( 'NONE',  ( -0.9982196940171965682, 0.000000000000000000, 0.05964429961207161346 ) ) ;
#14090 = AXIS2_PLACEMENT_3D ( 'NONE', #4927, #2541, #7242 ) ;
#14091 = VERTEX_POINT ( 'NONE', #13632 ) ;
#14092 = ORIENTED_EDGE ( 'NONE', *, *, #5981, .T. ) ;
#14093 = CARTESIAN_POINT ( 'NONE',  ( 38.25296960060453699, 0.000000000000000000, 42.65758570601131794 ) ) ;
#14094 = CARTESIAN_POINT ( 'NONE',  ( -4.592425496802573972E-16, 3.500000000000000000, -7.249999999999999112 ) ) ;
#14095 = CARTESIAN_POINT ( 'NONE',  ( -4.592425496802573972E-16, 5.999999999999999112, -7.250000000000000000 ) ) ;
#14096 = CARTESIAN_POINT ( 'NONE',  ( 0.7552767017676234040, 15.00000000000000000, -110.7727649483481400 ) ) ;
#14097 = ORIENTED_EDGE ( 'NONE', *, *, #5137, .F. ) ;
#14098 = CARTESIAN_POINT ( 'NONE',  ( -3.249999999999999556, 14.18750000000000000, -2.153805922287440833 ) ) ;
#14099 = CIRCLE ( 'NONE', #4463, 7.428243039713066764 ) ;
#14100 = AXIS2_PLACEMENT_3D ( 'NONE', #11925, #12001, #9380 ) ;
#14101 = CARTESIAN_POINT ( 'NONE',  ( -52.78575432782729848, 15.00000000000000000, -155.3001835197910907 ) ) ;
#14102 = VECTOR ( 'NONE', #10223, 1000.000000000000000 ) ;
#14103 = CARTESIAN_POINT ( 'NONE',  ( 3.289302641759264567, 8.673617379884035472E-16, -113.8917107963726494 ) ) ;
#14104 =( NAMED_UNIT ( * ) SI_UNIT ( $, .STERADIAN. ) SOLID_ANGLE_UNIT ( ) );
#14105 = CARTESIAN_POINT ( 'NONE',  ( 3.249999999999998668, 3.687500000000000444, -4.846194077712560500 ) ) ;
#14106 = COORDINATED_UNIVERSAL_TIME_OFFSET ( 0, 0, .AHEAD. ) ;
#14107 = CARTESIAN_POINT ( 'NONE',  ( 1.893911505664648054, 9.999999999999998224, -1.663006917529762152 ) ) ;
#14108 = CARTESIAN_POINT ( 'NONE',  ( 9.410602039359995175, 5.000000000000000888, -119.1126025277838920 ) ) ;
#14109 = ORIENTED_EDGE ( 'NONE', *, *, #2433, .F. ) ;
#14110 = CARTESIAN_POINT ( 'NONE',  ( -6.917334924218488723, 14.99999999999999822, -128.7878144224694950 ) ) ;
#14111 = CARTESIAN_POINT ( 'NONE',  ( -3.249999999999999556, 13.18750000000000000, -2.153805922287440833 ) ) ;
#14112 = VECTOR ( 'NONE', #4256, 1000.000000000000114 ) ;
#14113 = ORIENTED_EDGE ( 'NONE', *, *, #7824, .T. ) ;
#14114 = VERTEX_POINT ( 'NONE', #15025 ) ;
#14115 = CARTESIAN_POINT ( 'NONE',  ( 26.17093350124943640, 15.00000000000000000, -137.7213801722282085 ) ) ;
#14116 = CARTESIAN_POINT ( 'NONE',  ( -4.592425496802573972E-16, 6.000000000000000888, -7.250000000000000000 ) ) ;
#14117 = CARTESIAN_POINT ( 'NONE',  ( 3.249999999999998224, 6.187500000000001776, -4.846194077712561388 ) ) ;
#14118 = ORIENTED_EDGE ( 'NONE', *, *, #1446, .T. ) ;
#14119 = CARTESIAN_POINT ( 'NONE',  ( -0.3214635615754074527, 14.99999999999918998, -103.0394908280536299 ) ) ;
#14120 = CARTESIAN_POINT ( 'NONE',  ( 2.298097038856278473, 1.625000000000000222, -5.798097038856279362 ) ) ;
#14121 = PRODUCT ( 'ShearsLockingLatch_Predeterminado', 'ShearsLockingLatch_Predeterminado', '', ( #380 ) ) ;
#14122 = CARTESIAN_POINT ( 'NONE',  ( 1.553300858899105963, 10.56250000000000000, -7.250000000000000888 ) ) ;
#14123 = AXIS2_PLACEMENT_3D ( 'NONE', #7474, #9725, #453 ) ;
#14124 = CARTESIAN_POINT ( 'NONE',  ( -25.24442296148506770, 1.715658728670576227, -207.5621366369104237 ) ) ;
#14125 = CARTESIAN_POINT ( 'NONE',  ( 4.386720528383036388, -4.561518438557346199E-46, -133.8326913415544368 ) ) ;
#14126 = CARTESIAN_POINT ( 'NONE',  ( 7.722366886286562426, 14.99999999999999645, -107.3067671354286574 ) ) ;
#14127 = APPROVAL_STATUS ( 'not_yet_approved' ) ;
#14128 = DIRECTION ( 'NONE',  ( 0.000000000000000000, -1.000000000000000000, 0.000000000000000000 ) ) ;
#14129 = ORIENTED_EDGE ( 'NONE', *, *, #10253, .T. ) ;
#14130 = EDGE_CURVE ( 'NONE', #10677, #12952, #7744, .T. ) ;
#14131 = CARTESIAN_POINT ( 'NONE',  ( -3.249999999999999112, 7.812500000000000000, -4.846194077712558723 ) ) ;
#14132 = AXIS2_PLACEMENT_3D ( 'NONE', #8288, #339, #3896 ) ;
#14133 = CARTESIAN_POINT ( 'NONE',  ( -11.27598888897756702, 1.020558061026469510, -40.77697206847461331 ) ) ;
#14134 = CARTESIAN_POINT ( 'NONE',  ( -4.592425496802573972E-16, 12.00000000000000178, -7.250000000000000000 ) ) ;
#14135 = CARTESIAN_POINT ( 'NONE',  ( 4.999999999999998224, 0.000000000000000000, -45.97309604003007877 ) ) ;
#14136 = CARTESIAN_POINT ( 'NONE',  ( -65.68254623362582834, 14.99155785633053384, -190.1707496129446611 ) ) ;
#14137 = DIRECTION ( 'NONE',  ( 1.000000000000000000, 0.000000000000000000, 0.000000000000000000 ) ) ;
#14138 = CARTESIAN_POINT ( 'NONE',  ( 3.749999999999999556, 14.25000000000000178, -3.500000000000000444 ) ) ;
#14139 = CARTESIAN_POINT ( 'NONE',  ( 6.049910241306248437, 0.000000000000000000, -118.3734240199295300 ) ) ;
#14140 = APPROVAL_STATUS ( 'not_yet_approved' ) ;
#14141 = CARTESIAN_POINT ( 'NONE',  ( 2.298097038856279362, 14.87500000000000178, -1.201902961143720860 ) ) ;
#14142 = CARTESIAN_POINT ( 'NONE',  ( 6.422699671861707316, -4.000000000000000000, -139.1645012375703061 ) ) ;
#14143 = ORIENTED_EDGE ( 'NONE', *, *, #8852, .F. ) ;
#14144 = ADVANCED_FACE ( 'NONE', ( #5421 ), #2829, .T. ) ;
#14145 = CARTESIAN_POINT ( 'NONE',  ( -23.15133049553021749, 8.673617379884035472E-16, -203.9554707965373268 ) ) ;
#14146 = CARTESIAN_POINT ( 'NONE',  ( 2.298097038856278473, 1.625000000000000222, -5.798097038856279362 ) ) ;
#14147 = AXIS2_PLACEMENT_3D ( 'NONE', #3940, #1541, #14543 ) ;
#14148 = ADVANCED_FACE ( 'NONE', ( #11815, #13061 ), #15252, .F. ) ;
#14149 = CARTESIAN_POINT ( 'NONE',  ( -58.73854075889047976, 14.99999999999204370, -181.3184243507722613 ) ) ;
#14150 = CARTESIAN_POINT ( 'NONE',  ( 2.298097038856278029, 8.125000000000000000, -5.798097038856279362 ) ) ;
#14151 = ORIENTED_EDGE ( 'NONE', *, *, #10521, .F. ) ;
#14152 = CARTESIAN_POINT ( 'NONE',  ( -5.997216956047667580, 15.00000000000000000, -109.1002327432083945 ) ) ;
#14153 =( BOUNDED_SURFACE ( )  B_SPLINE_SURFACE ( 3, 3, ( 
 ( #11209, #630, #1551, #14554, #3951, #5335, #8654 ),
 ( #13389, #2793, #6342, #9897, #10630, #7803, #15293 ),
 ( #4683, #1932, #6721, #9399, #2297, #3089, #8235 ),
 ( #5909, #12516, #3444, #2009, #1202, #12963, #51 ) ),
 .UNSPECIFIED., .F., .F., .T. ) 
 B_SPLINE_SURFACE_WITH_KNOTS ( ( 4, 4 ),
 ( 4, 3, 4 ),
 ( 0.000000000000000000, 1.000000000000000000 ),
 ( 0.000000000000000000, 0.5000000000000000000, 1.000000000000000000 ),
 .UNSPECIFIED. ) 
 GEOMETRIC_REPRESENTATION_ITEM ( )  RATIONAL_B_SPLINE_SURFACE ( (
 ( 1.000000000000000000, 0.7662986988867873661, 0.7662986988867873661, 1.000000000000000000, 0.7662986988867873661, 0.7662986988867873661, 1.000000000000000000),
 ( 0.6468719831415924437, 0.4956971590277181594, 0.4956971590277181594, 0.6468719831415924437, 0.4956971590277181594, 0.4956971590277181594, 0.6468719831415924437),
 ( 0.6468719831415924437, 0.4956971590277181594, 0.4956971590277181594, 0.6468719831415924437, 0.4956971590277181594, 0.4956971590277181594, 0.6468719831415924437),
 ( 1.000000000000000000, 0.7662986988867873661, 0.7662986988867873661, 1.000000000000000000, 0.7662986988867873661, 0.7662986988867873661, 1.000000000000000000) ) ) 
 REPRESENTATION_ITEM ( '' )  SURFACE ( )  );
#14154 = CARTESIAN_POINT ( 'NONE',  ( 3.891364641103949307, 14.90536770052033688, -1.768596708628434211 ) ) ;
#14155 = CARTESIAN_POINT ( 'NONE',  ( 8.807773658240529713, 15.00000000000000000, -105.8689255569511261 ) ) ;
#14156 = CARTESIAN_POINT ( 'NONE',  ( 2.298097038856279362, 0.8750000000000000000, -1.201902961143720860 ) ) ;
#14157 = CARTESIAN_POINT ( 'NONE',  ( 1.346194077712561166, 12.43750000000000000, -0.2500000000000011102 ) ) ;
#14158 = CARTESIAN_POINT ( 'NONE',  ( 0.000000000000000000, 6.000000000000000000, 0.2500000000000002220 ) ) ;
#14159 = CARTESIAN_POINT ( 'NONE',  ( 0.2518559594811072277, 0.3124778193275194460, -7.146945437571262438 ) ) ;
#14160 = CARTESIAN_POINT ( 'NONE',  ( -2.651650429449552870, 3.625000000000000888, -0.8483495705504463524 ) ) ;
#14161 = VECTOR ( 'NONE', #8695, 1000.000000000000000 ) ;
#14162 = CARTESIAN_POINT ( 'NONE',  ( 30.32986759126112730, 0.7500000000000000000, 39.54214087805579680 ) ) ;
#14163 = CARTESIAN_POINT ( 'NONE',  ( -3.803627870483841100, 11.02901697934978031, -44.28669749208544459 ) ) ;
#14164 = LINE ( 'NONE', #4499, #13270 ) ;
#14165 = CARTESIAN_POINT ( 'NONE',  ( 7.113306724408225534, 0.000000000000000000, 51.45871142768356066 ) ) ;
#14166 = CARTESIAN_POINT ( 'NONE',  ( 3.249999999999999556, 10.75000000000000000, -3.500000000000000000 ) ) ;
#14167 = EDGE_CURVE ( 'NONE', #9845, #6034, #8265, .T. ) ;
#14168 = CARTESIAN_POINT ( 'NONE',  ( 39.42664711868611960, 1.750000000000000000, 42.16864325401552804 ) ) ;
#14169 = CARTESIAN_POINT ( 'NONE',  ( -64.47248607232361906, 14.98344778719946291, -184.4559935446063434 ) ) ;
#14170 = VERTEX_POINT ( 'NONE', #13933 ) ;
#14171 = EDGE_LOOP ( 'NONE', ( #128, #9425, #4749, #14241 ) ) ;
#14172 = CARTESIAN_POINT ( 'NONE',  ( -3.049680038147720484, 4.336808689942017736E-16, -109.9638061509243272 ) ) ;
#14173 = CARTESIAN_POINT ( 'NONE',  ( 10.36432819098247826, 8.673617379884035472E-16, -162.3272978866452831 ) ) ;
#14174 = CARTESIAN_POINT ( 'NONE',  ( 1.553300858899105963, 5.562500000000000000, -7.250000000000000888 ) ) ;
#14175 = CIRCLE ( 'NONE', #3543, 5.000000000000004441 ) ;
#14176 = CARTESIAN_POINT ( 'NONE',  ( 2.651650429449552870, 3.125000000000000444, -6.151650429449553314 ) ) ;
#14177 = CARTESIAN_POINT ( 'NONE',  ( 6.049910241306251990, 15.00000000000000000, -118.3734240199295300 ) ) ;
#14178 = ORIENTED_EDGE ( 'NONE', *, *, #1492, .T. ) ;
#14179 = CARTESIAN_POINT ( 'NONE',  ( -3.980102097228897245E-16, 13.50000000000000000, -6.749999999999999112 ) ) ;
#14180 = CARTESIAN_POINT ( 'NONE',  ( -0.7311112071359822107, 5.000000000000000888, -104.2753208119123798 ) ) ;
#14181 = FACE_OUTER_BOUND ( 'NONE', #8366, .T. ) ;
#14182 = CARTESIAN_POINT ( 'NONE',  ( 0.000000000000000000, 0.000000000000000000, 0.000000000000000000 ) ) ;
#14183 = CARTESIAN_POINT ( 'NONE',  ( -1.346194077712559389, 3.437500000000000000, -6.749999999999999112 ) ) ;
#14184 = APPROVAL_ROLE ( '' ) ;
#14185 = DIRECTION ( 'NONE',  ( 0.000000000000000000, 0.000000000000000000, -1.000000000000000000 ) ) ;
#14186 = CARTESIAN_POINT ( 'NONE',  ( 8.694046762582464893, 5.000000000000000888, -116.9683691483771071 ) ) ;
#14187 = VERTEX_POINT ( 'NONE', #10517 ) ;
#14188 = EDGE_CURVE ( 'NONE', #7422, #10346, #6957, .T. ) ;
#14189 = DIRECTION ( 'NONE',  ( 5.478074134663627674E-15, 0.000000000000000000, -1.000000000000000000 ) ) ;
#14190 = CARTESIAN_POINT ( 'NONE',  ( 0.000000000000000000, 15.00000000000000000, -0.2500000000000002220 ) ) ;
#14191 = VERTEX_POINT ( 'NONE', #1162 ) ;
#14192 = EDGE_LOOP ( 'NONE', ( #12412, #1655, #12078, #13750 ) ) ;
#14193 = CARTESIAN_POINT ( 'NONE',  ( -28.96136453847324788, 4.000000000000000000, -203.1938628845618666 ) ) ;
#14194 = CARTESIAN_POINT ( 'NONE',  ( -2.651650429449553314, 5.875000000000001776, -6.151650429449552426 ) ) ;
#14195 = CARTESIAN_POINT ( 'NONE',  ( -3.249999999999999556, 6.750000000000001776, -3.500000000000000000 ) ) ;
#14196 = ORIENTED_EDGE ( 'NONE', *, *, #45, .F. ) ;
#14197 = CARTESIAN_POINT ( 'NONE',  ( -0.06526978517727491380, 15.00000000000080824, -101.7940732946851341 ) ) ;
#14198 = CIRCLE ( 'NONE', #8013, 3.000000000000005329 ) ;
#14199 = CARTESIAN_POINT ( 'NONE',  ( -3.249999999999999556, 2.312500000000000888, -4.846194077712557835 ) ) ;
#14200 = CARTESIAN_POINT ( 'NONE',  ( -5.390763419087000408, 2.500000000000000444, -115.8096991919675673 ) ) ;
#14201 = CARTESIAN_POINT ( 'NONE',  ( -51.48498151979637782, 10.00000000000000000, -167.0076196043950745 ) ) ;
#14202 = DIRECTION ( 'NONE',  ( 1.000000000000000000, 0.000000000000000000, 0.000000000000000000 ) ) ;
#14203 = APPROVAL_STATUS ( 'not_yet_approved' ) ;
#14204 = DIRECTION ( 'NONE',  ( -0.9997619372588931741, -0.000000000000000000, -0.02181900108494707821 ) ) ;
#14205 = EDGE_LOOP ( 'NONE', ( #12182, #7830, #6598, #1348 ) ) ;
#14206 = DIRECTION ( 'NONE',  ( -0.9961255586397050887, 0.000000000000000000, 0.08794243244723005948 ) ) ;
#14207 = CARTESIAN_POINT ( 'NONE',  ( 1.553300858899109071, 13.43750000000000355, 0.2499999999999989175 ) ) ;
#14208 = DIRECTION ( 'NONE',  ( -0.7575874476598363216, 0.000000000000000000, -0.6527336816407245390 ) ) ;
#14209 = EDGE_CURVE ( 'NONE', #2112, #4560, #15143, .T. ) ;
#14210 = CARTESIAN_POINT ( 'NONE',  ( -64.84685337185132425, 15.24184988518138084, -207.0200216268500810 ) ) ;
#14211 = CARTESIAN_POINT ( 'NONE',  ( 3.890350893699057178, 9.999999999999998224, -1.782295516753907849 ) ) ;
#14212 = CARTESIAN_POINT ( 'NONE',  ( -3.980102097228897738E-16, 4.000000000000000888, -6.749999999999999112 ) ) ;
#14213 = CARTESIAN_POINT ( 'NONE',  ( 9.840588386097030238, 1.638247714399438948, -106.5338866644818125 ) ) ;
#14214 = APPLICATION_PROTOCOL_DEFINITION ( 'international standard', 'config_control_design', 1994, #81 ) ;
#14215 = CARTESIAN_POINT ( 'NONE',  ( -33.91109452335874153, 10.00000000000000178, -156.1716796081737471 ) ) ;
#14216 = DIRECTION ( 'NONE',  ( 0.000000000000000000, 0.000000000000000000, 1.000000000000000000 ) ) ;
#14217 = B_SPLINE_CURVE_WITH_KNOTS ( 'NONE', 3,
 ( #2968, #10299, #13720, #1890, #7680, #10155, #8840, #7833, #4211, #10234, #7900, #2039, #12547, #11161, #6750, #10007, #658, #4431 ),
 .UNSPECIFIED., .F., .F.,
 ( 4, 2, 2, 2, 2, 2, 2, 2, 4 ),
 ( 0.000000000000000000, 0.004943569348125147721, 0.007415354022187737627, 0.009887138696250326667, 0.01235892337031291484, 0.01359481570734420892, 0.01483070804437550301, 0.01730249271843805128, 0.01977427739250060129 ),
 .UNSPECIFIED. ) ;
#14218 = B_SPLINE_CURVE_WITH_KNOTS ( 'NONE', 3,
 ( #6008, #9808, #14294, #4856, #1617, #14465, #14539, #3861, #3694, #7324, #10733, #217, #12036, #9567, #13295, #6164, #8403, #2698, #7247, #2546, #4933, #12120, #1538, #6252, #10968, #1766, #7632, #766, #1920, #5394, #11113, #3006 ),
 .UNSPECIFIED., .F., .F.,
 ( 4, 2, 2, 2, 2, 2, 2, 2, 2, 2, 2, 2, 2, 2, 2, 4 ),
 ( 0.000000000000000000, 0.004332673798796619555, 0.008665347597593239110, 0.01299802139638985866, 0.01733069519518647822, 0.02599604279277973121, 0.03466139039037297725, 0.04332673798796622677, 0.04549307488736457211, 0.04765941178676291051, 0.05199208558555958731, 0.05632475938435627105, 0.06065743318315294785, 0.06499010698194963853, 0.06715644388134797693, 0.06932278078074631533 ),
 .UNSPECIFIED. ) ;
#14219 = ORIENTED_EDGE ( 'NONE', *, *, #532, .T. ) ;
#14220 = CARTESIAN_POINT ( 'NONE',  ( 7.149317070426778997, 1.131903150115492362, 1.667266480437773257 ) ) ;
#14221 = CARTESIAN_POINT ( 'NONE',  ( -3.249999999999999556, 3.187500000000000444, -2.153805922287440833 ) ) ;
#14222 = CARTESIAN_POINT ( 'NONE',  ( -61.97126637937648752, 15.00000000000265032, -193.9440536784921960 ) ) ;
#14223 = CARTESIAN_POINT ( 'NONE',  ( 2.298097038856278029, 6.125000000000000000, -5.798097038856279362 ) ) ;
#14224 = VERTEX_POINT ( 'NONE', #14078 ) ;
#14225 = CARTESIAN_POINT ( 'NONE',  ( -0.1096517733176519821, 15.00000000000000000, -113.0403960504791314 ) ) ;
#14226 = UNCERTAINTY_MEASURE_WITH_UNIT (LENGTH_MEASURE( 1.000000000000000082E-05 ), #5521, 'distance_accuracy_value', 'NONE');
#14227 = CARTESIAN_POINT ( 'NONE',  ( 17.37339609381778871, 6.000000000000000000, -130.0984517650821886 ) ) ;
#14228 = CARTESIAN_POINT ( 'NONE',  ( -0.3498759111043971970, 15.00000000000000000, -139.6126861214085011 ) ) ;
#14229 = CARTESIAN_POINT ( 'NONE',  ( -3.249999999999999556, 2.187500000000000444, -2.153805922287440833 ) ) ;
#14230 = CARTESIAN_POINT ( 'NONE',  ( 1.553300858899105963, 2.062500000000000000, -7.249999999999999112 ) ) ;
#14231 = CARTESIAN_POINT ( 'NONE',  ( 3.749999999999999556, 3.812500000000000000, -1.946699141100892261 ) ) ;
#14232 = CARTESIAN_POINT ( 'NONE',  ( 5.475206276408092876, 0.000000000000000000, -34.56909192082981974 ) ) ;
#14233 = CARTESIAN_POINT ( 'NONE',  ( -3.750000000000000000, 7.687500000000000888, -1.946699141100893149 ) ) ;
#14234 = CARTESIAN_POINT ( 'NONE',  ( 4.703427927161452970, 14.48245223617349531, 1.488206399065538532 ) ) ;
#14235 = EDGE_CURVE ( 'NONE', #13676, #9933, #5225, .T. ) ;
#14236 = CARTESIAN_POINT ( 'NONE',  ( -3.822077182119589800, 11.22755171044550160, -45.02879370139852711 ) ) ;
#14237 = CARTESIAN_POINT ( 'NONE',  ( -7.791963050599854945, 0.3085994142892563574, -104.8053269544278123 ) ) ;
#14238 = CARTESIAN_POINT ( 'NONE',  ( -3.249999999999999556, 13.31250000000000000, -4.846194077712557835 ) ) ;
#14239 = CARTESIAN_POINT ( 'NONE',  ( 2.752881441477233349, 5.000000000000000888, 2.754251355355158193 ) ) ;
#14240 = DIRECTION ( 'NONE',  ( 0.08794243244723005948, 0.000000000000000000, 0.9961255586397049777 ) ) ;
#14241 = ORIENTED_EDGE ( 'NONE', *, *, #2836, .F. ) ;
#14242 = ORIENTED_EDGE ( 'NONE', *, *, #1166, .F. ) ;
#14243 = CARTESIAN_POINT ( 'NONE',  ( -3.665430453447521497, 4.336808689942017736E-16, -108.2557784285269946 ) ) ;
#14244 = LINE ( 'NONE', #11686, #3768 ) ;
#14245 = CARTESIAN_POINT ( 'NONE',  ( 3.750000000000000000, 4.750000000000000000, -3.500000000000000444 ) ) ;
#14246 = CARTESIAN_POINT ( 'NONE',  ( 3.749999999999999556, 4.249999999999999112, -3.500000000000000444 ) ) ;
#14247 = DIRECTION ( 'NONE',  ( -0.000000000000000000, 1.000000000000000000, -0.000000000000000000 ) ) ;
#14248 = ORIENTED_EDGE ( 'NONE', *, *, #9712, .F. ) ;
#14249 = ADVANCED_BREP_SHAPE_REPRESENTATION ( '', ( #7440, #9419 ), #6228 ) ;
#14250 = CARTESIAN_POINT ( 'NONE',  ( -3.249999999999999112, 5.687500000000000888, -2.153805922287440833 ) ) ;
#14251 = B_SPLINE_CURVE_WITH_KNOTS ( 'NONE', 3,
 ( #1494, #180, #11764, #4664, #10764, #29, #14330, #13170, #2501, #4892, #2351, #8287, #14257, #15270, #2580, #9531, #7280, #3586, #11994, #14103, #7196, #9602, #1418, #6123, #4970, #7049, #3504, #4818, #9685, #14417 ),
 .UNSPECIFIED., .F., .F.,
 ( 4, 2, 2, 2, 2, 2, 2, 2, 2, 2, 2, 2, 2, 2, 4 ),
 ( 6.938893903907228378E-18, 0.005155083077057498811, 0.007732624615586275105, 0.01031016615411505313, 0.01546524923117260572, 0.02062033230823015831, 0.02319787384675891725, 0.02577541538528767620, 0.02835295692381643515, 0.03093049846234519409, 0.03350804000087395651, 0.03479681077013833251, 0.03608558153940271546, 0.03866312307793146746, 0.04124066461646022641 ),
 .UNSPECIFIED. ) ;
#14252 = EDGE_CURVE ( 'NONE', #6217, #5312, #5946, .T. ) ;
#14253 = CIRCLE ( 'NONE', #12271, 5.000000000000000888 ) ;
#14254 = CARTESIAN_POINT ( 'NONE',  ( -0.3803025174127598884, 5.000000000000000888, -103.2080563861792655 ) ) ;
#14255 = EDGE_CURVE ( 'NONE', #12952, #5739, #4866, .T. ) ;
#14256 = EDGE_CURVE ( 'NONE', #12868, #8964, #10136, .T. ) ;
#14257 = CARTESIAN_POINT ( 'NONE',  ( 5.703550681602465922, 8.673617379884033500E-16, -122.9904140605998890 ) ) ;
#14258 = CARTESIAN_POINT ( 'NONE',  ( -2.298097038856278918, 7.375000000000000888, -5.798097038856277585 ) ) ;
#14259 = CARTESIAN_POINT ( 'NONE',  ( 0.000000000000000000, 1.000000000000000000, 0.000000000000000000 ) ) ;
#14260 = SECURITY_CLASSIFICATION_LEVEL ( 'unclassified' ) ;
#14261 = DIRECTION ( 'NONE',  ( -0.000000000000000000, -1.000000000000000000, -0.000000000000000000 ) ) ;
#14262 = CARTESIAN_POINT ( 'NONE',  ( 10.27130088872558211, 5.000000000000000888, -120.9123952259834027 ) ) ;
#14263 = ORIENTED_EDGE ( 'NONE', *, *, #12258, .F. ) ;
#14264 = CARTESIAN_POINT ( 'NONE',  ( -0.1986981485396748237, 15.00000000000000000, -111.2607621713454193 ) ) ;
#14265 = CARTESIAN_POINT ( 'NONE',  ( -2.298097038856278918, 13.37500000000000000, -5.798097038856277585 ) ) ;
#14266 = ORIENTED_EDGE ( 'NONE', *, *, #1240, .F. ) ;
#14267 = VERTEX_POINT ( 'NONE', #6021 ) ;
#14268 = CARTESIAN_POINT ( 'NONE',  ( -30.30611677948249039, 4.000000000000000888, -198.2470835936195783 ) ) ;
#14269 = CARTESIAN_POINT ( 'NONE',  ( 1.553300858899105963, 5.062500000000000000, -7.250000000000000888 ) ) ;
#14270 = CARTESIAN_POINT ( 'NONE',  ( -3.249999999999999112, 8.812500000000001776, -4.846194077712558723 ) ) ;
#14271 = VERTEX_POINT ( 'NONE', #10742 ) ;
#14272 = CARTESIAN_POINT ( 'NONE',  ( -2.424117392948417216, 9.999999999999998224, -107.6599666633534866 ) ) ;
#14273 = CARTESIAN_POINT ( 'NONE',  ( 3.249999999999998668, 1.687500000000000000, -4.846194077712560500 ) ) ;
#14274 = CARTESIAN_POINT ( 'NONE',  ( -10.86141109878643718, 2.499999999999999556, -125.6973785677633373 ) ) ;
#14275 = CARTESIAN_POINT ( 'NONE',  ( 13.01561562359685276, 3.439206092960765293, -166.0850505222445008 ) ) ;
#14276 = PERSON_AND_ORGANIZATION ( #3176, #3020 ) ;
#14277 = CARTESIAN_POINT ( 'NONE',  ( 11.00225911879145002, 8.749999999999998224, -91.84275802117696230 ) ) ;
#14278 = VERTEX_POINT ( 'NONE', #157 ) ;
#14279 = CARTESIAN_POINT ( 'NONE',  ( 7.995229681650334541, 1.921202954650395700, -34.56909192082981974 ) ) ;
#14280 = CARTESIAN_POINT ( 'NONE',  ( -1.553300858899106629, 14.56250000000000000, 0.2499999999999998335 ) ) ;
#14281 = CARTESIAN_POINT ( 'NONE',  ( 6.049910241306248437, 15.00000000000000000, -118.3734240199295300 ) ) ;
#14282 = CARTESIAN_POINT ( 'NONE',  ( -67.58669624565897038, 10.46432717369429888, -204.4673446941004045 ) ) ;
#14283 = CARTESIAN_POINT ( 'NONE',  ( 17.43525470771941599, 8.749999999999998224, -88.70164870234812327 ) ) ;
#14284 = CARTESIAN_POINT ( 'NONE',  ( -2.298097038856278029, 2.625000000000000000, -1.201902961143720638 ) ) ;
#14285 = CARTESIAN_POINT ( 'NONE',  ( 10.54544248586296717, 2.723356639041063953, -106.8702387211511819 ) ) ;
#14286 = COORDINATED_UNIVERSAL_TIME_OFFSET ( 0, 0, .AHEAD. ) ;
#14287 = CARTESIAN_POINT ( 'NONE',  ( 0.000000000000000000, 15.00000000000000000, -0.2500000000000002220 ) ) ;
#14288 = CARTESIAN_POINT ( 'NONE',  ( -0.4453226528549816265, -2.225540348348185052E-17, 1.000000000000000000 ) ) ;
#14289 = EDGE_CURVE ( 'NONE', #882, #602, #12766, .T. ) ;
#14290 = EDGE_LOOP ( 'NONE', ( #6387, #5584, #7534, #11540, #7295, #8871, #9588, #5320, #4806, #1005, #14760, #9343, #11283, #9146, #2150 ) ) ;
#14291 = CARTESIAN_POINT ( 'NONE',  ( 8.026035668590276728, 2.099780044019236236, 2.291639928401612014 ) ) ;
#14292 = CARTESIAN_POINT ( 'NONE',  ( 2.298097038856279362, 2.875000000000000000, -1.201902961143720860 ) ) ;
#14293 = EDGE_CURVE ( 'NONE', #11348, #12551, #1103, .T. ) ;
#14294 = CARTESIAN_POINT ( 'NONE',  ( -49.63713232248656482, 9.999999999999998224, -143.5380774856291168 ) ) ;
#14295 = CARTESIAN_POINT ( 'NONE',  ( -3.249999999999999556, 12.25000000000000000, -3.499999999999999556 ) ) ;
#14296 = CARTESIAN_POINT ( 'NONE',  ( -3.980102097228897245E-16, 11.50000000000000000, -6.749999999999999112 ) ) ;
#14297 = CARTESIAN_POINT ( 'NONE',  ( -3.249999999999999556, 5.750000000000000888, -3.500000000000000000 ) ) ;
#14298 = VERTEX_POINT ( 'NONE', #14305 ) ;
#14299 = CARTESIAN_POINT ( 'NONE',  ( -5.254015288425265773, 15.00000000000000178, -115.0648584343368555 ) ) ;
#14300 = CARTESIAN_POINT ( 'NONE',  ( 0.2625675448779695720, 9.999999999999998224, 2.974107436473218957 ) ) ;
#14301 = CARTESIAN_POINT ( 'NONE',  ( -4.827681327704948622, 9.999999999999998224, -144.0483944136971388 ) ) ;
#14302 = CARTESIAN_POINT ( 'NONE',  ( -1.346194077712559389, 0.4375000000000000555, -6.749999999999999112 ) ) ;
#14303 = CARTESIAN_POINT ( 'NONE',  ( -4.592425496802573972E-16, 1.000000000000000000, -7.250000000000000000 ) ) ;
#14304 = CARTESIAN_POINT ( 'NONE',  ( 1.553300858899105963, 3.562500000000000000, -7.250000000000000000 ) ) ;
#14305 = CARTESIAN_POINT ( 'NONE',  ( 51.16773099383375012, 0.000000000000000000, 70.62880098866567380 ) ) ;
#14306 = CARTESIAN_POINT ( 'NONE',  ( 3.750000000000000000, 4.312500000000000000, -1.946699141100892705 ) ) ;
#14307 = CARTESIAN_POINT ( 'NONE',  ( 0.9668478293219275876, 12.62857015536147998, 2.475663031890364962 ) ) ;
#14308 = CARTESIAN_POINT ( 'NONE',  ( 9.520855056337145683, 1.077704823981404338E-10, -163.5635978942416102 ) ) ;
#14309 = CARTESIAN_POINT ( 'NONE',  ( 1.167531179896771798, 4.000000000000000000, -139.4941991647475845 ) ) ;
#14310 = CARTESIAN_POINT ( 'NONE',  ( -3.868309323113294340, -5.416683946349036576E-13, -143.9840091578641363 ) ) ;
#14311 = CARTESIAN_POINT ( 'NONE',  ( -2.298097038856278473, 14.12500000000000000, -1.201902961143720416 ) ) ;
#14312 = CARTESIAN_POINT ( 'NONE',  ( 6.766120961959584790, 0.8459668203398081898, 1.356709294556286860 ) ) ;
#14313 = FACE_OUTER_BOUND ( 'NONE', #10298, .T. ) ;
#14314 = EDGE_LOOP ( 'NONE', ( #6894, #15008, #3076, #13886, #12568, #10728 ) ) ;
#14315 = LOCAL_TIME ( 12, 28, 20.00000000000000000, #7378 ) ;
#14316 = ADVANCED_FACE ( 'NONE', ( #14630 ), #7045, .T. ) ;
#14317 = CARTESIAN_POINT ( 'NONE',  ( 1.553300858899109516, 10.43750000000000178, 0.2499999999999993616 ) ) ;
#14318 = ORIENTED_EDGE ( 'NONE', *, *, #4680, .T. ) ;
#14319 = CARTESIAN_POINT ( 'NONE',  ( -6.038383048961361688, 2.500000000000000444, -118.0543633390209806 ) ) ;
#14320 = CARTESIAN_POINT ( 'NONE',  ( -24.55211425566311689, 2.243498015498064377E-12, -206.7125218406129079 ) ) ;
#14321 = CARTESIAN_POINT ( 'NONE',  ( -1.553300858899107295, 10.43750000000000000, -7.250000000000000000 ) ) ;
#14322 = CARTESIAN_POINT ( 'NONE',  ( 3.749999999999999112, 3.312500000000000000, -1.946699141100893149 ) ) ;
#14323 = VECTOR ( 'NONE', #11079, 1000.000000000000000 ) ;
#14324 = CARTESIAN_POINT ( 'NONE',  ( -17.99773676121543176, 1.745015017355616038, -129.4573227159242776 ) ) ;
#14325 = ORIENTED_EDGE ( 'NONE', *, *, #15123, .T. ) ;
#14326 = CARTESIAN_POINT ( 'NONE',  ( -7.230043083586494390, 0.9058721943649702402, -116.2995594653100682 ) ) ;
#14327 = CARTESIAN_POINT ( 'NONE',  ( 0.000000000000000000, 4.499999999999999112, -0.2500000000000002220 ) ) ;
#14328 = CARTESIAN_POINT ( 'NONE',  ( -59.94788933422542954, 9.999999999999998224, -157.3141654284602851 ) ) ;
#14329 = CC_DESIGN_APPROVAL ( #548, ( #8149 ) ) ;
#14330 = CARTESIAN_POINT ( 'NONE',  ( 13.55522405627131910, 8.673617379884037444E-16, -133.0209701713156392 ) ) ;
#14331 = CC_DESIGN_PERSON_AND_ORGANIZATION_ASSIGNMENT ( #5150, #1519, ( #8377 ) ) ;
#14332 =( NAMED_UNIT ( * ) PLANE_ANGLE_UNIT ( ) SI_UNIT ( $, .RADIAN. ) );
#14333 = CARTESIAN_POINT ( 'NONE',  ( 3.249999999999998668, 9.687500000000000000, -4.846194077712560500 ) ) ;
#14334 = CIRCLE ( 'NONE', #8899, 9.800000000000252953 ) ;
#14335 = DIRECTION ( 'NONE',  ( 0.000000000000000000, 0.9434476287765544145, 0.3315216007380165641 ) ) ;
#14336 = CARTESIAN_POINT ( 'NONE',  ( -6.451063615512949490, -8.037239669988805559E-13, -125.7472547710006694 ) ) ;
#14337 = CARTESIAN_POINT ( 'NONE',  ( 9.374169689979092723, 8.673617379884035472E-16, -128.5794221292618431 ) ) ;
#14338 = ORIENTED_EDGE ( 'NONE', *, *, #3836, .T. ) ;
#14339 = CARTESIAN_POINT ( 'NONE',  ( -2.133154950264692040, 15.00000000000000711, -105.7915708274213955 ) ) ;
#14340 = CARTESIAN_POINT ( 'NONE',  ( 3.249999999999999556, 13.75000000000000000, -3.500000000000000000 ) ) ;
#14341 = VERTEX_POINT ( 'NONE', #11205 ) ;
#14342 = EDGE_CURVE ( 'NONE', #13160, #7022, #7723, .T. ) ;
#14343 = ORIENTED_EDGE ( 'NONE', *, *, #8346, .T. ) ;
#14344 = DIRECTION ( 'NONE',  ( 1.000000000000000000, 0.000000000000000000, 0.000000000000000000 ) ) ;
#14345 = CARTESIAN_POINT ( 'NONE',  ( 2.651650429449554203, 4.375000000000000888, -0.8483495705504471296 ) ) ;
#14346 = EDGE_CURVE ( 'NONE', #13403, #8964, #14593, .T. ) ;
#14347 = CARTESIAN_POINT ( 'NONE',  ( -2.298097038856278029, 9.624999999999998224, -1.201902961143720638 ) ) ;
#14349 = EDGE_CURVE ( 'NONE', #1764, #6135, #3126, .T. ) ;
#14348 = ORIENTED_EDGE ( 'NONE', *, *, #2712, .T. ) ;
#14350 = AXIS2_PLACEMENT_3D ( 'NONE', #12502, #535, #10192 ) ;
#14351 = CARTESIAN_POINT ( 'NONE',  ( -3.768042520815404917, 9.999999999999998224, -109.5986228335790145 ) ) ;
#14352 = VECTOR ( 'NONE', #8741, 1000.000000000000227 ) ;
#14353 = CARTESIAN_POINT ( 'NONE',  ( -3.249999999999999556, 5.250000000000000000, -3.499999999999999556 ) ) ;
#14354 = AXIS2_PLACEMENT_3D ( 'NONE', #1862, #11433, #8961 ) ;
#14355 = CIRCLE ( 'NONE', #10388, 7.000000000000000000 ) ;
#14356 = CARTESIAN_POINT ( 'NONE',  ( -5.344111538902212466, 2.500000000000000444, -111.1470454227235365 ) ) ;
#14357 = CARTESIAN_POINT ( 'NONE',  ( 12.73427191684880277, 2.644333132995618119, -165.8787509141178020 ) ) ;
#14358 = CARTESIAN_POINT ( 'NONE',  ( -0.2500000000000000555, 5.000000000000000000, -1.499999999999999778 ) ) ;
#14359 = DATE_AND_TIME ( #3999, #8133 ) ;
#14360 = CIRCLE ( 'NONE', #4724, 9.800000000000252953 ) ;
#14361 = PLANE ( 'NONE',  #1099 ) ;
#14362 = EDGE_LOOP ( 'NONE', ( #6281, #13291, #10268 ) ) ;
#14363 = CARTESIAN_POINT ( 'NONE',  ( 2.298097038856279362, 9.875000000000000000, -1.201902961143720860 ) ) ;
#14364 = CARTESIAN_POINT ( 'NONE',  ( 0.000000000000000000, 13.50000000000000178, -0.2500000000000002220 ) ) ;
#14365 = EDGE_CURVE ( 'NONE', #14224, #14065, #7946, .T. ) ;
#14366 = CC_DESIGN_PERSON_AND_ORGANIZATION_ASSIGNMENT ( #10631, #3303, ( #11099 ) ) ;
#14367 = CARTESIAN_POINT ( 'NONE',  ( -3.812461735095854287, 15.00000000000000178, -118.8814295322933390 ) ) ;
#14368 =( GEOMETRIC_REPRESENTATION_CONTEXT ( 3 ) GLOBAL_UNCERTAINTY_ASSIGNED_CONTEXT ( ( #634 ) ) GLOBAL_UNIT_ASSIGNED_CONTEXT ( ( #8357, #8595, #9603 ) ) REPRESENTATION_CONTEXT ( 'NONE', 'WORKASPACE' ) );
#14369 = CARTESIAN_POINT ( 'NONE',  ( 1.553300858899105963, 12.06250000000000000, -7.249999999999999112 ) ) ;
#14370 = CARTESIAN_POINT ( 'NONE',  ( -63.51383849574869345, 11.85838142801650186, -202.9177410002877764 ) ) ;
#14371 = CARTESIAN_POINT ( 'NONE',  ( 14.17108320694883972, 12.64090008863623460, -126.4473401621325763 ) ) ;
#14372 = CARTESIAN_POINT ( 'NONE',  ( 3.249999999999998224, 3.187500000000000444, -4.846194077712561388 ) ) ;
#14373 = CARTESIAN_POINT ( 'NONE',  ( 10.78057029805192180, 2.723356638990212186, -106.2467252071195389 ) ) ;
#14374 = APPROVAL_ROLE ( '' ) ;
#14375 = DIRECTION ( 'NONE',  ( 0.000000000000000000, 0.000000000000000000, 1.000000000000000000 ) ) ;
#14376 = CARTESIAN_POINT ( 'NONE',  ( 1.243260443319662123, 6.000000000000000000, -139.4020581015306846 ) ) ;
#14377 = LOCAL_TIME ( 12, 28, 20.00000000000000000, #14063 ) ;
#14378 = ORIENTED_EDGE ( 'NONE', *, *, #4158, .T. ) ;
#14379 = CARTESIAN_POINT ( 'NONE',  ( 5.742112159410722505, 2.751696591659712698, 4.680416356127273581 ) ) ;
#14380 = CARTESIAN_POINT ( 'NONE',  ( 1.346194077712560944, 8.937500000000001776, -0.2500000000000011102 ) ) ;
#14381 = CARTESIAN_POINT ( 'NONE',  ( -9.147714614026110524, 1.812406719287864121, -104.6428665161372749 ) ) ;
#14382 = CARTESIAN_POINT ( 'NONE',  ( -2.298097038856278918, 12.37500000000000000, -5.798097038856277585 ) ) ;
#14383 = CARTESIAN_POINT ( 'NONE',  ( -1.346194077712559167, 7.937500000000001776, -6.749999999999999112 ) ) ;
#14384 = CARTESIAN_POINT ( 'NONE',  ( -5.574230463510377653, 14.99999999999939604, -116.5593450232588424 ) ) ;
#14385 = DIRECTION ( 'NONE',  ( 0.000000000000000000, 0.000000000000000000, 1.000000000000000000 ) ) ;
#14386 = DIRECTION ( 'NONE',  ( 0.5205261093005589812, 0.000000000000000000, -0.8538457527776445177 ) ) ;
#14387 = CARTESIAN_POINT ( 'NONE',  ( 3.249999999999999556, 2.750000000000000000, -3.500000000000000000 ) ) ;
#14388 = CARTESIAN_POINT ( 'NONE',  ( -2.651650429449552870, 0.8750000000000000000, -6.151650429449552426 ) ) ;
#14389 = CARTESIAN_POINT ( 'NONE',  ( -2.651650429449553314, 5.375000000000000000, -6.151650429449552426 ) ) ;
#14390 = APPROVAL_PERSON_ORGANIZATION ( #7476, #6183, #6323 ) ;
#14391 = CARTESIAN_POINT ( 'NONE',  ( 0.1752993268022353945, 3.004311909859588070, 1.985618716487552726 ) ) ;
#14392 = CARTESIAN_POINT ( 'NONE',  ( -3.750000000000000000, 6.687500000000000888, -1.946699141100893149 ) ) ;
#14393 = CARTESIAN_POINT ( 'NONE',  ( 4.414185141403890178, 14.05584352489653632, 2.594153855646779583 ) ) ;
#14394 = CARTESIAN_POINT ( 'NONE',  ( 9.500324903962138023, 2.296263824619149852E-15, -163.5886270269263889 ) ) ;
#14395 = AXIS2_PLACEMENT_3D ( 'NONE', #3960, #8822, #7506 ) ;
#14396 = LINE ( 'NONE', #1470, #11324 ) ;
#14397 = CARTESIAN_POINT ( 'NONE',  ( 1.078231930479242484, 6.000000000000000000, -139.4303258909232852 ) ) ;
#14398 = CARTESIAN_POINT ( 'NONE',  ( -0.3766621274091715987, 0.5000000000000000000, 0.1491815183709511716 ) ) ;
#14399 = B_SPLINE_CURVE_WITH_KNOTS ( 'NONE', 3,
 ( #10078, #13500, #5434, #7757, #14813, #12546, #10154, #4210, #8991, #11387, #4139, #8839, #5217, #4067, #13644, #9928 ),
 .UNSPECIFIED., .F., .F.,
 ( 4, 2, 2, 2, 2, 2, 2, 4 ),
 ( 0.000000000000000000, 0.0004968996385939453836, 0.0009937992771878907672, 0.001490698915781836151, 0.001987598554375781534, 0.002484498192969726918, 0.002981397831563672302, 0.003975197108751563069 ),
 .UNSPECIFIED. ) ;
#14400 = CARTESIAN_POINT ( 'NONE',  ( -1.870253773668272945, 8.673617379884035472E-16, -147.6241727244333504 ) ) ;
#14401 = PLANE ( 'NONE',  #12334 ) ;
#14402 = VERTEX_POINT ( 'NONE', #776 ) ;
#14403 = CARTESIAN_POINT ( 'NONE',  ( -1.553300858899107073, 10.93750000000000000, -7.249999999999999112 ) ) ;
#14404 = EDGE_LOOP ( 'NONE', ( #14668, #74, #9835, #240, #14694, #2038, #14895, #8312, #10933, #6994, #4227, #12852, #10735 ) ) ;
#14405 = CARTESIAN_POINT ( 'NONE',  ( -6.701857729407779019, 2.500000000000000444, -119.5348842627718398 ) ) ;
#14406 = CARTESIAN_POINT ( 'NONE',  ( 5.137957026085648415, -1.921202954650397476, -45.03258396026099319 ) ) ;
#14407 = CARTESIAN_POINT ( 'NONE',  ( 2.651650429449552870, 10.62500000000000000, -6.151650429449554203 ) ) ;
#14408 = CARTESIAN_POINT ( 'NONE',  ( 2.651650429449552870, 8.125000000000000000, -6.151650429449553314 ) ) ;
#14409 = CARTESIAN_POINT ( 'NONE',  ( -17.94289163462782710, 1.572396511098281158, -129.5251036616920430 ) ) ;
#14410 = ORIENTED_EDGE ( 'NONE', *, *, #5243, .F. ) ;
#14411 = CARTESIAN_POINT ( 'NONE',  ( -6.777586278698636946, 0.5200622811955745162, -116.7594943224618191 ) ) ;
#14412 = AXIS2_PLACEMENT_3D ( 'NONE', #3296, #8938, #13667 ) ;
#14413 = CARTESIAN_POINT ( 'NONE',  ( 3.249999999999999556, 5.249999999999999112, -3.500000000000000000 ) ) ;
#14414 = EDGE_CURVE ( 'NONE', #9908, #15055, #13688, .T. ) ;
#14415 = CARTESIAN_POINT ( 'NONE',  ( 1.553300858899105963, 8.562500000000001776, -7.250000000000000888 ) ) ;
#14416 = CARTESIAN_POINT ( 'NONE',  ( -69.17701953972918716, 14.99999999999999645, -200.3386666625191879 ) ) ;
#14417 = CARTESIAN_POINT ( 'NONE',  ( 6.288457687488933523, 0.000000000000000000, -105.0111312234435985 ) ) ;
#14418 = EDGE_CURVE ( 'NONE', #14267, #1356, #8884, .T. ) ;
#14419 = CARTESIAN_POINT ( 'NONE',  ( -3.249999999999999556, 7.312500000000000888, -4.846194077712557835 ) ) ;
#14420 = PLANE ( 'NONE',  #4623 ) ;
#14421 = COORDINATED_UNIVERSAL_TIME_OFFSET ( 0, 0, .AHEAD. ) ;
#14422 = CARTESIAN_POINT ( 'NONE',  ( -7.251835631666873283, 7.915809026670424014E-13, -123.8995801872388824 ) ) ;
#14423 = CARTESIAN_POINT ( 'NONE',  ( 19.51808381319401065, 4.284816698714185730E-13, -131.6416685808667069 ) ) ;
#14424 = ORIENTED_EDGE ( 'NONE', *, *, #9025, .T. ) ;
#14425 = VECTOR ( 'NONE', #11989, 1000.000000000000227 ) ;
#14426 = DIRECTION ( 'NONE',  ( -0.000000000000000000, 1.000000000000000000, -0.000000000000000000 ) ) ;
#14427 = VECTOR ( 'NONE', #6881, 1000.000000000000000 ) ;
#14428 = CARTESIAN_POINT ( 'NONE',  ( 0.2499999999999999445, 4.500000000000000888, -0.2499999999999997780 ) ) ;
#14429 = ORIENTED_EDGE ( 'NONE', *, *, #5368, .F. ) ;
#14430 = ORIENTED_EDGE ( 'NONE', *, *, #8870, .F. ) ;
#14431 = CARTESIAN_POINT ( 'NONE',  ( 23.38516724735982777, 0.4291895315141152634, -138.6768690072186700 ) ) ;
#14432 = CARTESIAN_POINT ( 'NONE',  ( -1.553300858899106629, 14.56250000000000000, 0.2499999999999998335 ) ) ;
#14433 = CARTESIAN_POINT ( 'NONE',  ( -3.249999999999999112, 6.812500000000000000, -4.846194077712558723 ) ) ;
#14434 = CC_DESIGN_PERSON_AND_ORGANIZATION_ASSIGNMENT ( #12341, #12575, ( #8454 ) ) ;
#14435 = CARTESIAN_POINT ( 'NONE',  ( -2.298097038856279362, 11.87500000000000000, -5.798097038856278473 ) ) ;
#14436 = ORIENTED_EDGE ( 'NONE', *, *, #1668, .T. ) ;
#14437 = CARTESIAN_POINT ( 'NONE',  ( -3.768042520875636292, 15.00000000000000000, -109.5986228335309391 ) ) ;
#14438 = CARTESIAN_POINT ( 'NONE',  ( 2.298097038856278473, 5.625000000000000000, -5.798097038856279362 ) ) ;
#14439 = CIRCLE ( 'NONE', #2822, 3.500000000000000000 ) ;
#14440 = VECTOR ( 'NONE', #10130, 1000.000000000000000 ) ;
#14441 = CARTESIAN_POINT ( 'NONE',  ( -5.125635908759425874, 2.499999999999999556, -112.7029199983815602 ) ) ;
#14442 = EDGE_CURVE ( 'NONE', #11957, #4481, #12512, .T. ) ;
#14443 = CARTESIAN_POINT ( 'NONE',  ( -57.93401690343701205, 10.00000000000000178, -179.1696213049108053 ) ) ;
#14444 = DIRECTION ( 'NONE',  ( 0.000000000000000000, 1.000000000000000000, 0.000000000000000000 ) ) ;
#14445 = EDGE_CURVE ( 'NONE', #13806, #3650, #9899, .T. ) ;
#14446 = DATE_AND_TIME ( #13351, #8881 ) ;
#14447 = LINE ( 'NONE', #11027, #1344 ) ;
#14448 = ORIENTED_EDGE ( 'NONE', *, *, #4158, .F. ) ;
#14449 = CARTESIAN_POINT ( 'NONE',  ( -2.298097038856278918, 0.3750000000000000000, -5.798097038856277585 ) ) ;
#14450 = AXIS2_PLACEMENT_3D ( 'NONE', #9478, #15225, #4839 ) ;
#14451 = CARTESIAN_POINT ( 'NONE',  ( 1.553300858899105963, 11.56249999999999822, -7.250000000000000888 ) ) ;
#14452 = DIRECTION ( 'NONE',  ( 0.000000000000000000, 1.000000000000000000, 0.000000000000000000 ) ) ;
#14453 = CARTESIAN_POINT ( 'NONE',  ( 0.000000000000000000, 13.50000000000000355, 0.2499999999999998057 ) ) ;
#14454 = CARTESIAN_POINT ( 'NONE',  ( -67.62515672639226239, 11.98211585291473469, -203.5224559347309992 ) ) ;
#14455 = FACE_OUTER_BOUND ( 'NONE', #350, .T. ) ;
#14456 = CARTESIAN_POINT ( 'NONE',  ( -3.249999999999999112, 1.687500000000000222, -2.153805922287440833 ) ) ;
#14457 = CARTESIAN_POINT ( 'NONE',  ( 8.711870733155482327, 0.6047360044100810184, -105.8325059764879370 ) ) ;
#14458 = EDGE_CURVE ( 'NONE', #11635, #750, #2005, .T. ) ;
#14459 = COORDINATED_UNIVERSAL_TIME_OFFSET ( 0, 0, .AHEAD. ) ;
#14460 = DIRECTION ( 'NONE',  ( 0.000000000000000000, 0.000000000000000000, 1.000000000000000000 ) ) ;
#14461 = CARTESIAN_POINT ( 'NONE',  ( -0.2500000000000000555, 4.500000000000000888, 1.500000000000000222 ) ) ;
#14462 = ORIENTED_EDGE ( 'NONE', *, *, #12738, .F. ) ;
#14463 = CARTESIAN_POINT ( 'NONE',  ( 6.082631124755410568, 0.4612449235174558293, 0.6929822686081172911 ) ) ;
#14464 = CARTESIAN_POINT ( 'NONE',  ( 0.000000000000000000, 9.000000000000001776, -0.2500000000000002220 ) ) ;
#14465 = CARTESIAN_POINT ( 'NONE',  ( -54.39630486114151608, 9.999999999999996447, -148.9727485570832926 ) ) ;
#14466 = CARTESIAN_POINT ( 'NONE',  ( 3.249999999999998668, 14.68750000000000000, -4.846194077712560500 ) ) ;
#14467 = CARTESIAN_POINT ( 'NONE',  ( -3.249999999999999556, 9.750000000000000000, -3.500000000000000000 ) ) ;
#14468 = CARTESIAN_POINT ( 'NONE',  ( -7.267596910904561724, 9.999999999999998224, -107.1579542029217720 ) ) ;
#14469 = CARTESIAN_POINT ( 'NONE',  ( -0.2510664901725777054, -0.2041261725989376163, -0.1347136637304948981 ) ) ;
#14470 = CARTESIAN_POINT ( 'NONE',  ( 8.807773658237110226, 15.00000000000000000, -105.8689255569501171 ) ) ;
#14471 = CARTESIAN_POINT ( 'NONE',  ( -1.346194077712559389, 3.437500000000000000, -6.749999999999999112 ) ) ;
#14472 = CARTESIAN_POINT ( 'NONE',  ( 3.749999999999998668, 2.187500000000000000, -5.053300858899108405 ) ) ;
#14473 = CARTESIAN_POINT ( 'NONE',  ( -4.592425496802573972E-16, 5.500000000000000000, -7.249999999999999112 ) ) ;
#14474 = CARTESIAN_POINT ( 'NONE',  ( -3.910513648578280321, 11.22738257010117557, -46.03033150271466667 ) ) ;
#14475 = CARTESIAN_POINT ( 'NONE',  ( -4.592425496802573972E-16, 8.000000000000000000, -7.250000000000000000 ) ) ;
#14476 = CARTESIAN_POINT ( 'NONE',  ( 4.086606960750444273, 13.49296761167366476, 3.472055327930651636 ) ) ;
#14477 = CARTESIAN_POINT ( 'NONE',  ( 13.14021484082229030, 4.050274393866083678, -166.1764203671933444 ) ) ;
#14478 =( BOUNDED_SURFACE ( )  B_SPLINE_SURFACE ( 3, 2, ( 
 ( #7020, #1154, #10576 ),
 ( #9423, #12983, #15315 ),
 ( #3549, #11516, #931 ),
 ( #11044, #9649, #14620 ),
 ( #11883, #460, #5018 ),
 ( #13052, #3937, #7397 ),
 ( #5095, #6086, #1457 ),
 ( #386, #304, #8638 ),
 ( #5170, #13218, #1306 ),
 ( #1385, #9882, #4018 ),
 ( #14381, #2464, #3780 ),
 ( #9736, #13135, #11961 ),
 ( #146, #13374, #12201 ),
 ( #2779, #6329, #7483 ) ),
 .UNSPECIFIED., .F., .F., .F. ) 
 B_SPLINE_SURFACE_WITH_KNOTS ( ( 4, 2, 2, 2, 2, 2, 4 ),
 ( 3, 3 ),
 ( -8.724106040071283679E-06, 0.0006126034624112808996, 0.001233931030862633156, 0.001544594815088309175, 0.001855258599313985412, 0.002165922383539661648, 0.002476586167765337451 ),
 ( 0.000000000000000000, 1.000000000000000000 ),
 .UNSPECIFIED. ) 
 GEOMETRIC_REPRESENTATION_ITEM ( )  RATIONAL_B_SPLINE_SURFACE ( (
 ( 1.000000000000000000, 1.000000000000000000, 1.000000000000000000),
 ( 1.000000000000000000, 0.9999955273081105878, 1.000000000000000000),
 ( 1.000000000000000000, 0.9954486024702557945, 1.000000000000000000),
 ( 1.000000000000000000, 0.9776029025031673925, 1.000000000000000000),
 ( 1.000000000000000000, 0.9647625072224111920, 1.000000000000000000),
 ( 1.000000000000000000, 0.9425905009577734139, 1.000000000000000000),
 ( 1.000000000000000000, 0.9349995798840151640, 1.000000000000000000),
 ( 1.000000000000000000, 0.9203396985081793158, 1.000000000000000000),
 ( 1.000000000000000000, 0.9132096254797749113, 1.000000000000000000),
 ( 1.000000000000000000, 0.9008818398987329390, 1.000000000000000000),
 ( 1.000000000000000000, 0.8958246136694008044, 1.000000000000000000),
 ( 1.000000000000000000, 0.8888068886117856948, 1.000000000000000000),
 ( 1.000000000000000000, 0.8868507700907835023, 1.000000000000000000),
 ( 1.000000000000000000, 0.8868705507870304761, 1.000000000000000000) ) ) 
 REPRESENTATION_ITEM ( '' )  SURFACE ( )  );
#14479 = DIRECTION ( 'NONE',  ( -0.000000000000000000, 1.000000000000000000, 0.000000000000000000 ) ) ;
#14480 = CARTESIAN_POINT ( 'NONE',  ( -4.375735311315418485, 3.999999999999874767, -143.3439008670868020 ) ) ;
#14481 = CARTESIAN_POINT ( 'NONE',  ( -25.68053481550299111, 15.00000000000000000, -142.4798935003980773 ) ) ;
#14482 = CARTESIAN_POINT ( 'NONE',  ( -25.78682146806830033, 8.673617379884035472E-16, -192.1400676150700804 ) ) ;
#14483 = CARTESIAN_POINT ( 'NONE',  ( 4.047901359269184596, 1.717432757859984984E-11, -106.4041221357184668 ) ) ;
#14484 = VERTEX_POINT ( 'NONE', #4108 ) ;
#14485 = CARTESIAN_POINT ( 'NONE',  ( 2.651650429449554203, 10.37500000000000000, -0.8483495705504471296 ) ) ;
#14486 = ORIENTED_EDGE ( 'NONE', *, *, #6065, .T. ) ;
#14487 = CARTESIAN_POINT ( 'NONE',  ( -5.223664414336186113, 2.500000000000000444, -111.8183263698799266 ) ) ;
#14488 = CARTESIAN_POINT ( 'NONE',  ( -10.29275726619094300, 0.000000000000000000, -34.56909192082969895 ) ) ;
#14489 = CARTESIAN_POINT ( 'NONE',  ( -1.553300858899106629, 9.062499999999998224, 0.2500000000000002220 ) ) ;
#14490 = CARTESIAN_POINT ( 'NONE',  ( -2.651650429449552870, 7.625000000000000000, -0.8483495705504467965 ) ) ;
#14491 = CARTESIAN_POINT ( 'NONE',  ( 0.000000000000000000, 0.000000000000000000, 0.000000000000000000 ) ) ;
#14492 = ORIENTED_EDGE ( 'NONE', *, *, #5993, .F. ) ;
#14493 = CARTESIAN_POINT ( 'NONE',  ( -8.923457816048948388, 2.191178284877700833, -116.0747321664481717 ) ) ;
#14494 = CARTESIAN_POINT ( 'NONE',  ( -3.980102097228897738E-16, 4.000000000000000000, -6.749999999999999112 ) ) ;
#14495 = CARTESIAN_POINT ( 'NONE',  ( -3.750000000000000000, 10.25000000000000000, -3.499999999999999112 ) ) ;
#14496 = CARTESIAN_POINT ( 'NONE',  ( -67.50271866739358018, 14.99999999999315037, -175.2102855836816673 ) ) ;
#14497 = CARTESIAN_POINT ( 'NONE',  ( -47.48189921986828210, 9.999999999999998224, -141.5723758807981483 ) ) ;
#14498 = CARTESIAN_POINT ( 'NONE',  ( 3.249999999999998668, 7.687500000000000000, -4.846194077712560500 ) ) ;
#14499 = DIRECTION ( 'NONE',  ( 0.000000000000000000, 1.000000000000000000, -0.000000000000000000 ) ) ;
#14500 = CONTEXT_DEPENDENT_SHAPE_REPRESENTATION ( #9266, #13991 ) ;
#14501 = CARTESIAN_POINT ( 'NONE',  ( -8.326762664983050399, -7.864679486792610604E-13, -121.0857513972968604 ) ) ;
#14502 = CARTESIAN_POINT ( 'NONE',  ( 8.300023318284271312, -4.283195660063827066E-13, -113.4762057881885795 ) ) ;
#14503 = VERTEX_POINT ( 'NONE', #8809 ) ;
#14504 = DIRECTION ( 'NONE',  ( 0.000000000000000000, 0.000000000000000000, -1.000000000000000000 ) ) ;
#14505 = DIRECTION ( 'NONE',  ( 0.000000000000000000, 0.000000000000000000, 1.000000000000000000 ) ) ;
#14506 = ORIENTED_EDGE ( 'NONE', *, *, #14544, .T. ) ;
#14507 = EDGE_CURVE ( 'NONE', #14984, #9311, #4411, .T. ) ;
#14508 = ORIENTED_EDGE ( 'NONE', *, *, #4694, .F. ) ;
#14509 = DIRECTION ( 'NONE',  ( 0.000000000000000000, 0.000000000000000000, -1.000000000000000000 ) ) ;
#14510 = CARTESIAN_POINT ( 'NONE',  ( -3.749999999999999556, 11.75000000000000178, -3.499999999999999112 ) ) ;
#14511 = CARTESIAN_POINT ( 'NONE',  ( 1.346194077712558279, 11.06250000000000178, -6.750000000000000888 ) ) ;
#14512 = CARTESIAN_POINT ( 'NONE',  ( -3.249999999999999556, 9.750000000000000000, -3.500000000000000000 ) ) ;
#14513 = ORIENTED_EDGE ( 'NONE', *, *, #12686, .T. ) ;
#14514 = EDGE_CURVE ( 'NONE', #2651, #12098, #8921, .T. ) ;
#14515 = CARTESIAN_POINT ( 'NONE',  ( -9.476787056091271921, 9.999999999999998224, -115.4301398046334981 ) ) ;
#14516 = CARTESIAN_POINT ( 'NONE',  ( 3.249999999999999556, 7.750000000000000000, -3.500000000000000000 ) ) ;
#14517 = CARTESIAN_POINT ( 'NONE',  ( -25.43320932775275978, 3.897330828535134017, -209.0242640618165808 ) ) ;
#14518 = CARTESIAN_POINT ( 'NONE',  ( 10.23189628017364505, 0.1924065811658746683, -164.0445219108954973 ) ) ;
#14519 = FACE_OUTER_BOUND ( 'NONE', #15206, .T. ) ;
#14520 = SECURITY_CLASSIFICATION_LEVEL ( 'unclassified' ) ;
#14521 = DIRECTION ( 'NONE',  ( 0.000000000000000000, 0.000000000000000000, -1.000000000000000000 ) ) ;
#14522 = ORIENTED_EDGE ( 'NONE', *, *, #2595, .F. ) ;
#14523 = CARTESIAN_POINT ( 'NONE',  ( 0.000000000000000000, 10.00000000000000000, -0.2500000000000002220 ) ) ;
#14524 = CARTESIAN_POINT ( 'NONE',  ( -2.298097038856279362, 13.87500000000000178, -5.798097038856278473 ) ) ;
#14525 = CARTESIAN_POINT ( 'NONE',  ( 2.651650429449553759, 14.87500000000000178, -0.8483495705504471296 ) ) ;
#14526 = EDGE_CURVE ( 'NONE', #11140, #5472, #12820, .T. ) ;
#14527 = DIRECTION ( 'NONE',  ( 0.000000000000000000, 0.000000000000000000, -1.000000000000000000 ) ) ;
#14528 = CARTESIAN_POINT ( 'NONE',  ( -2.651650429449553314, 1.375000000000000000, -6.151650429449552426 ) ) ;
#14529 = CARTESIAN_POINT ( 'NONE',  ( -64.78057553730850771, 15.17580650425065514, -207.3219553479909507 ) ) ;
#14530 = CARTESIAN_POINT ( 'NONE',  ( -0.3766621274091715987, 0.2398196381212478467, -0.1347136637304948426 ) ) ;
#14531 = CARTESIAN_POINT ( 'NONE',  ( 9.114992375658264478, 0.8572809181108925758, -105.9776340796685332 ) ) ;
#14532 = PERSON_AND_ORGANIZATION ( #3176, #3020 ) ;
#14533 = DIRECTION ( 'NONE',  ( -0.000000000000000000, 1.000000000000000000, -0.000000000000000000 ) ) ;
#14534 = DIRECTION ( 'NONE',  ( 0.000000000000000000, 1.000000000000000000, 0.000000000000000000 ) ) ;
#14535 = CC_DESIGN_PERSON_AND_ORGANIZATION_ASSIGNMENT ( #3277, #9228, ( #3971 ) ) ;
#14536 = ORIENTED_EDGE ( 'NONE', *, *, #5630, .F. ) ;
#14537 = CARTESIAN_POINT ( 'NONE',  ( 8.409813745801482554, 2.751696592305300282, 2.538033216846526940 ) ) ;
#14538 = CARTESIAN_POINT ( 'NONE',  ( 2.298097038856279362, 6.875000000000000000, -1.201902961143720860 ) ) ;
#14539 = CARTESIAN_POINT ( 'NONE',  ( -55.26439141815399836, 9.999999999999998224, -150.1289833821797970 ) ) ;
#14540 = CARTESIAN_POINT ( 'NONE',  ( -3.249999999999999556, 12.18750000000000000, -2.153805922287440833 ) ) ;
#14541 = EDGE_CURVE ( 'NONE', #11999, #5680, #12160, .T. ) ;
#14542 = CARTESIAN_POINT ( 'NONE',  ( -1.346194077712558945, 10.56249999999999822, -0.2500000000000002220 ) ) ;
#14543 = DIRECTION ( 'NONE',  ( 0.000000000000000000, 0.000000000000000000, -1.000000000000000000 ) ) ;
#14544 = EDGE_CURVE ( 'NONE', #3281, #8227, #12122, .T. ) ;
#14545 = CARTESIAN_POINT ( 'NONE',  ( -2.298097038856278918, 0.3750000000000000000, -5.798097038856277585 ) ) ;
#14546 = EDGE_CURVE ( 'NONE', #3511, #10578, #5346, .T. ) ;
#14547 = DIRECTION ( 'NONE',  ( -0.9961255586397049777, -0.000000000000000000, 0.08794243244723005948 ) ) ;
#14548 = CARTESIAN_POINT ( 'NONE',  ( -2.298097038856278473, 4.125000000000000000, -1.201902961143720416 ) ) ;
#14549 = CARTESIAN_POINT ( 'NONE',  ( 3.749999999999999556, 3.250000000000000000, -3.500000000000000444 ) ) ;
#14550 = CARTESIAN_POINT ( 'NONE',  ( -3.750000000000000000, 10.18750000000000000, -1.946699141100892927 ) ) ;
#14551 = CARTESIAN_POINT ( 'NONE',  ( 0.05457537653413515460, 2.500000000000001332, 0.6181762992656862910 ) ) ;
#14552 = CARTESIAN_POINT ( 'NONE',  ( -3.749999999999999556, 7.750000000000000888, -3.499999999999999112 ) ) ;
#14553 = CARTESIAN_POINT ( 'NONE',  ( 1.476973400873566433, 13.35568666265236537, 2.081368828687825800 ) ) ;
#14554 = CARTESIAN_POINT ( 'NONE',  ( -0.5793326530874193248, -2.075239479414269894, -43.47630266472464911 ) ) ;
#14555 = CARTESIAN_POINT ( 'NONE',  ( 7.788671722263528885, 7.321094445766561876, -20.36947622874119546 ) ) ;
#14556 = CARTESIAN_POINT ( 'NONE',  ( -2.515578278476028107, 8.673617379884035472E-16, -148.1512477234490177 ) ) ;
#14557 = CARTESIAN_POINT ( 'NONE',  ( 2.298097038856278473, 14.62500000000000000, -5.798097038856279362 ) ) ;
#14558 = PLANE ( 'NONE',  #3711 ) ;
#14559 = ORIENTED_EDGE ( 'NONE', *, *, #7883, .F. ) ;
#14560 = CARTESIAN_POINT ( 'NONE',  ( -4.592425496802573972E-16, 13.00000000000000000, -7.250000000000000000 ) ) ;
#14561 = VERTEX_POINT ( 'NONE', #992 ) ;
#14562 = DIRECTION ( 'NONE',  ( 0.000000000000000000, -0.000000000000000000, 1.000000000000000000 ) ) ;
#14563 = CARTESIAN_POINT ( 'NONE',  ( 12.67805275830794898, 8.673617379884037444E-16, -154.9658299924666665 ) ) ;
#14564 = CARTESIAN_POINT ( 'NONE',  ( -2.651650429449552870, 9.125000000000000000, -0.8483495705504462414 ) ) ;
#14565 = CARTESIAN_POINT ( 'NONE',  ( -2.651650429449552870, 7.874999999999999112, -6.151650429449552426 ) ) ;
#14566 = CARTESIAN_POINT ( 'NONE',  ( -3.190623165655964488, 7.379999999999996341, -41.82578512943236149 ) ) ;
#14567 = ORIENTED_EDGE ( 'NONE', *, *, #14635, .T. ) ;
#14568 = CARTESIAN_POINT ( 'NONE',  ( 3.249999999999998224, 6.312500000000000000, -2.153805922287439945 ) ) ;
#14569 = CARTESIAN_POINT ( 'NONE',  ( 3.749999999999998668, 11.68750000000000000, -5.053300858899107517 ) ) ;
#14570 = CARTESIAN_POINT ( 'NONE',  ( -64.76906036162762348, 15.00000000000000000, -167.3305518093332296 ) ) ;
#14571 = DIRECTION ( 'NONE',  ( 3.540251991789310798E-15, 0.000000000000000000, -1.000000000000000000 ) ) ;
#14572 = CARTESIAN_POINT ( 'NONE',  ( -1.346194077712559389, 9.437500000000000000, -6.749999999999999112 ) ) ;
#14573 = FACE_OUTER_BOUND ( 'NONE', #1566, .T. ) ;
#14574 = DATE_AND_TIME ( #6210, #11107 ) ;
#14575 = CC_DESIGN_APPROVAL ( #3278, ( #7881 ) ) ;
#14576 = CARTESIAN_POINT ( 'NONE',  ( -5.134731047560421757, 1.592765399726224076E-12, -128.4544621779126885 ) ) ;
#14577 = CARTESIAN_POINT ( 'NONE',  ( 1.831246893856141034, 2.490287375297123962, -1.000000000000028644 ) ) ;
#14578 = ORIENTED_EDGE ( 'NONE', *, *, #13875, .T. ) ;
#14579 = AXIS2_PLACEMENT_3D ( 'NONE', #11259, #6391, #756 ) ;
#14580 = DIRECTION ( 'NONE',  ( -8.764770998266003672E-18, 0.000000000000000000, -1.000000000000000000 ) ) ;
#14581 = PLANE ( 'NONE',  #3950 ) ;
#14582 = EDGE_LOOP ( 'NONE', ( #9537, #13548 ) ) ;
#14583 = CARTESIAN_POINT ( 'NONE',  ( 27.03835354040201011, 4.628448260288817728, -138.2189567750509127 ) ) ;
#14584 = CARTESIAN_POINT ( 'NONE',  ( 2.651650429449553314, 13.37500000000000000, -0.8483495705504476847 ) ) ;
#14585 = CARTESIAN_POINT ( 'NONE',  ( -1.346194077712558945, 11.56250000000000178, -0.2500000000000002220 ) ) ;
#14586 = CARTESIAN_POINT ( 'NONE',  ( 2.298097038856278029, 12.12500000000000000, -5.798097038856279362 ) ) ;
#14587 = ORIENTED_EDGE ( 'NONE', *, *, #4956, .F. ) ;
#14588 = DIRECTION ( 'NONE',  ( 0.7575874476598363216, 0.000000000000000000, 0.6527336816407246500 ) ) ;
#14589 = CARTESIAN_POINT ( 'NONE',  ( 3.249999999999999112, 8.812500000000000000, -2.153805922287439945 ) ) ;
#14590 = LOCAL_TIME ( 12, 28, 20.00000000000000000, #6687 ) ;
#14591 = FACE_OUTER_BOUND ( 'NONE', #905, .T. ) ;
#14592 = VECTOR ( 'NONE', #10921, 1000.000000000000227 ) ;
#14593 = B_SPLINE_CURVE_WITH_KNOTS ( 'NONE', 3,
 ( #9034, #4398, #5258, #11428, #13539, #13759, #5554, #3154, #9107, #3017, #627, #6487, #15002, #8957, #12665, #1859, #4331, #850 ),
 .UNSPECIFIED., .F., .F.,
 ( 4, 2, 2, 2, 2, 2, 2, 2, 4 ),
 ( 0.000000000000000000, 0.001051779247122254166, 0.002103558494244507030, 0.003155337741366759895, 0.004207116988489012326, 0.005258896235611266491, 0.006310675482733521524, 0.007362454729855774822, 0.008414233976978029855 ),
 .UNSPECIFIED. ) ;
#14594 = CARTESIAN_POINT ( 'NONE',  ( 11.57097051246173969, 14.81307274914749961, -125.6777153510405185 ) ) ;
#14595 = DIRECTION ( 'NONE',  ( -0.000000000000000000, -1.000000000000000000, -0.000000000000000000 ) ) ;
#14596 = CARTESIAN_POINT ( 'NONE',  ( -3.688685944975817144, 7.379999999999996341, -41.78181391320875093 ) ) ;
#14597 = CALENDAR_DATE ( 2026, 8, 10 ) ;
#14598 = CARTESIAN_POINT ( 'NONE',  ( -26.78870578381917866, 5.000000000000000000, -139.1599602021251769 ) ) ;
#14599 = VECTOR ( 'NONE', #6132, 1000.000000000000000 ) ;
#14600 = VERTEX_POINT ( 'NONE', #4771 ) ;
#14601 = CARTESIAN_POINT ( 'NONE',  ( 3.249999999999999112, 0.8125000000000001110, -2.153805922287439945 ) ) ;
#14602 = CARTESIAN_POINT ( 'NONE',  ( -2.651650429449552870, 12.12500000000000000, -0.8483495705504462414 ) ) ;
#14603 = CIRCLE ( 'NONE', #13367, 5.000000000000000000 ) ;
#14604 = AXIS2_PLACEMENT_3D ( 'NONE', #3544, #2694, #10727 ) ;
#14605 = VERTEX_POINT ( 'NONE', #5703 ) ;
#14606 = CARTESIAN_POINT ( 'NONE',  ( -9.836272398077403167, -1.921202954650395478, -34.71741284551207229 ) ) ;
#14607 = CARTESIAN_POINT ( 'NONE',  ( 1.553300858899105963, 2.562500000000000444, -7.250000000000000888 ) ) ;
#14608 = AXIS2_PLACEMENT_3D ( 'NONE', #10002, #3824, #7287 ) ;
#14609 = DIRECTION ( 'NONE',  ( 0.000000000000000000, -1.000000000000000000, 0.000000000000000000 ) ) ;
#14610 = FACE_BOUND ( 'NONE', #2513, .T. ) ;
#14611 = CIRCLE ( 'NONE', #9902, 14.80000000000025651 ) ;
#14612 = CARTESIAN_POINT ( 'NONE',  ( -4.592425496802573972E-16, 1.500000000000000000, -7.249999999999999112 ) ) ;
#14613 = CALENDAR_DATE ( 2026, 8, 10 ) ;
#14614 = EDGE_CURVE ( 'NONE', #14051, #5529, #10422, .T. ) ;
#14615 = DIRECTION ( 'NONE',  ( 0.000000000000000000, 1.000000000000000000, 0.000000000000000000 ) ) ;
#14616 = CARTESIAN_POINT ( 'NONE',  ( 37.88191578704505957, 0.000000000000000000, 42.20832867525968624 ) ) ;
#14617 = APPLICATION_CONTEXT ( 'configuration controlled 3d designs of mechanical parts and assemblies' ) ;
#14618 = EDGE_LOOP ( 'NONE', ( #14118, #13661, #7806, #14109 ) ) ;
#14619 = CARTESIAN_POINT ( 'NONE',  ( -3.249999999999999556, 8.187500000000000000, -2.153805922287440833 ) ) ;
#14620 = CARTESIAN_POINT ( 'NONE',  ( -7.760546158192966892, 0.2897469121590799390, -104.7856241544137958 ) ) ;
#14621 = CARTESIAN_POINT ( 'NONE',  ( 3.249999999999999556, 13.75000000000000000, -3.500000000000000000 ) ) ;
#14622 = CIRCLE ( 'NONE', #7162, 2.000000000000007994 ) ;
#14623 = CARTESIAN_POINT ( 'NONE',  ( 1.346194077712558279, 11.06250000000000178, -6.750000000000000888 ) ) ;
#14624 = FACE_OUTER_BOUND ( 'NONE', #521, .T. ) ;
#14625 = DIRECTION ( 'NONE',  ( 0.000000000000000000, -1.000000000000000000, 0.000000000000000000 ) ) ;
#14626 = CARTESIAN_POINT ( 'NONE',  ( 1.243260443319662123, 4.179859613694246079, -139.4020581015306846 ) ) ;
#14627 = CARTESIAN_POINT ( 'NONE',  ( -3.249999999999999556, 3.312500000000000000, -4.846194077712557835 ) ) ;
#14628 = CARTESIAN_POINT ( 'NONE',  ( -3.749999999999999556, 6.750000000000000888, -3.499999999999999112 ) ) ;
#14629 = CARTESIAN_POINT ( 'NONE',  ( -2.651650429449552870, 8.125000000000000000, -0.8483495705504462414 ) ) ;
#14630 = FACE_OUTER_BOUND ( 'NONE', #5114, .T. ) ;
#14631 = CARTESIAN_POINT ( 'NONE',  ( 1.553300858899105963, 11.06250000000000178, -7.250000000000000888 ) ) ;
#14632 = CARTESIAN_POINT ( 'NONE',  ( 3.759523211377189700, 14.85715077771003578, -0.7426300787629251943 ) ) ;
#14633 = VECTOR ( 'NONE', #12962, 1000.000000000000000 ) ;
#14634 = CARTESIAN_POINT ( 'NONE',  ( 12.67258870470521614, 3.477781664713254894, -166.5210692261007637 ) ) ;
#14635 = EDGE_CURVE ( 'NONE', #4330, #13403, #5694, .T. ) ;
#14636 = EDGE_CURVE ( 'NONE', #4779, #6217, #13857, .T. ) ;
#14637 = CARTESIAN_POINT ( 'NONE',  ( 7.719042654902918521, 10.85333879869827278, -21.53480312112609596 ) ) ;
#14638 = CARTESIAN_POINT ( 'NONE',  ( -30.65815467000176042, 3.999999999999813483, -194.1257268749498337 ) ) ;
#14639 = CARTESIAN_POINT ( 'NONE',  ( 5.651020395687034181, 0.03103945442896835147, -140.5875639640649979 ) ) ;
#14640 = CARTESIAN_POINT ( 'NONE',  ( 8.935548306746159852, 4.627360597499654560, 2.855381328098121507 ) ) ;
#14641 = CARTESIAN_POINT ( 'NONE',  ( 0.000000000000000000, 0.5000000000000001110, -0.2500000000000002220 ) ) ;
#14642 = ORIENTED_EDGE ( 'NONE', *, *, #3349, .T. ) ;
#14643 = CARTESIAN_POINT ( 'NONE',  ( -0.01496453197141594735, 5.000000000000000000, -5.196130874293185542 ) ) ;
#14644 = CARTESIAN_POINT ( 'NONE',  ( -22.23979083886640851, 4.000000000000000000, -203.8707431750928833 ) ) ;
#14645 = CARTESIAN_POINT ( 'NONE',  ( 2.651650429449552870, 8.625000000000000000, -6.151650429449554203 ) ) ;
#14646 = CARTESIAN_POINT ( 'NONE',  ( -1.553300858899107073, 9.937500000000001776, -7.249999999999999112 ) ) ;
#14647 = ORIENTED_EDGE ( 'NONE', *, *, #3936, .F. ) ;
#14648 = LOCAL_TIME ( 12, 28, 20.00000000000000000, #8678 ) ;
#14649 = CARTESIAN_POINT ( 'NONE',  ( 3.249999999999998224, 7.187500000000000888, -4.846194077712561388 ) ) ;
#14650 = CARTESIAN_POINT ( 'NONE',  ( 2.651650429449552870, 8.625000000000000000, -6.151650429449554203 ) ) ;
#14651 = CARTESIAN_POINT ( 'NONE',  ( -67.78894975818599278, 14.99999999999827693, -204.1377247862654372 ) ) ;
#14652 = DIRECTION ( 'NONE',  ( 0.000000000000000000, -0.6972771395097939751, 0.7168016397282022112 ) ) ;
#14653 = CARTESIAN_POINT ( 'NONE',  ( 2.298097038856278473, 11.62500000000000000, -5.798097038856279362 ) ) ;
#14654 = ADVANCED_FACE ( 'NONE', ( #12974 ), #2378, .T. ) ;
#14655 = CARTESIAN_POINT ( 'NONE',  ( -6.483256266768061771, 10.00000000000000178, -108.2602118674242888 ) ) ;
#14656 = CARTESIAN_POINT ( 'NONE',  ( -0.1621610436782315590, 4.999999999999206857, -136.1940307094523632 ) ) ;
#14657 = CARTESIAN_POINT ( 'NONE',  ( 9.550372274932042771, 5.000000000000000888, -109.1178429856281156 ) ) ;
#14658 = LINE ( 'NONE', #13495, #10632 ) ;
#14659 = CARTESIAN_POINT ( 'NONE',  ( 0.2499999999999999445, 5.000000000000000000, 1.500000000000000222 ) ) ;
#14660 = VERTEX_POINT ( 'NONE', #14530 ) ;
#14661 = EDGE_CURVE ( 'NONE', #5270, #4145, #2762, .T. ) ;
#14662 = CARTESIAN_POINT ( 'NONE',  ( 8.895558325401111688, 6.000000000000000000, -141.4560052469132643 ) ) ;
#14663 = CARTESIAN_POINT ( 'NONE',  ( -0.01496453197141594735, 5.000000000000000000, -5.196130874293185542 ) ) ;
#14664 = CARTESIAN_POINT ( 'NONE',  ( -2.651650429449552870, 12.87500000000000178, -6.151650429449552426 ) ) ;
#14665 = CIRCLE ( 'NONE', #13911, 7.428243039713066764 ) ;
#14666 = CARTESIAN_POINT ( 'NONE',  ( 2.298097038856279362, 11.37500000000000178, -1.201902961143720860 ) ) ;
#14667 = CARTESIAN_POINT ( 'NONE',  ( 2.298097038856279362, 1.875000000000000000, -1.201902961143720860 ) ) ;
#14668 = ORIENTED_EDGE ( 'NONE', *, *, #10644, .F. ) ;
#14669 =( BOUNDED_CURVE ( )  B_SPLINE_CURVE ( 3, ( #14873, #1940, #7658, #7879 ),
 .UNSPECIFIED., .F., .F. ) 
 B_SPLINE_CURVE_WITH_KNOTS ( ( 4, 4 ),
 ( 0.1758562950254942969, 0.7234361084260857444 ),
 .UNSPECIFIED. ) 
 CURVE ( )  GEOMETRIC_REPRESENTATION_ITEM ( )  RATIONAL_B_SPLINE_CURVE ( ( 1.000000000000000000, 0.9751687266833821699, 0.9751687266833821699, 1.000000000000000000 ) ) 
 REPRESENTATION_ITEM ( '' )  );
#14670 = CARTESIAN_POINT ( 'NONE',  ( 3.249999999999999112, 7.812500000000000000, -2.153805922287439945 ) ) ;
#14671 = CARTESIAN_POINT ( 'NONE',  ( -5.309262520577839872, 6.000000000000000000, -125.0911079416483176 ) ) ;
#14672 = CARTESIAN_POINT ( 'NONE',  ( -5.309889193474533364, 14.88217507572605491, -103.7269406991748184 ) ) ;
#14673 = CARTESIAN_POINT ( 'NONE',  ( -25.14935590298316015, 3.999999999999999112, -209.2172623628708550 ) ) ;
#14674 = CARTESIAN_POINT ( 'NONE',  ( -39.71273995388224165, 15.00000000000000355, -151.9652294113466837 ) ) ;
#14675 = AXIS2_PLACEMENT_3D ( 'NONE', #2346, #2269, #5880 ) ;
#14676 = APPROVAL_STATUS ( 'not_yet_approved' ) ;
#14677 = AXIS2_PLACEMENT_3D ( 'NONE', #10403, #8858, #10318 ) ;
#14678 = FACE_OUTER_BOUND ( 'NONE', #6213, .T. ) ;
#14679 = EDGE_LOOP ( 'NONE', ( #11773, #8838, #14178, #14871 ) ) ;
#14680 = CARTESIAN_POINT ( 'NONE',  ( 3.249999999999999556, 0.7500000000000000000, -3.500000000000000000 ) ) ;
#14681 = CARTESIAN_POINT ( 'NONE',  ( 2.651650429449552870, 14.62500000000000000, -6.151650429449554203 ) ) ;
#14682 = EDGE_LOOP ( 'NONE', ( #1506, #14318, #11912, #11770 ) ) ;
#14683 = CARTESIAN_POINT ( 'NONE',  ( -4.878690035801932723, -1.020558061026469066, -0.3860167444088121180 ) ) ;
#14684 = AXIS2_PLACEMENT_3D ( 'NONE', #4717, #3553, #12987 ) ;
#14685 = AXIS2_PLACEMENT_3D ( 'NONE', #692, #9739, #3864 ) ;
#14686 = CARTESIAN_POINT ( 'NONE',  ( -3.749999999999999556, 2.312500000000000888, -5.053300858899104853 ) ) ;
#14687 = CARTESIAN_POINT ( 'NONE',  ( 7.301969087183287854, 3.176662348976181605, -22.75718819171553520 ) ) ;
#14688 = CARTESIAN_POINT ( 'NONE',  ( 0.4942027541975256288, 3.793956966360130689, 5.597843736040499785 ) ) ;
#14689 = CARTESIAN_POINT ( 'NONE',  ( 1.553300858899105963, 2.562500000000000444, -7.250000000000000000 ) ) ;
#14690 = MECHANICAL_CONTEXT ( 'NONE', #4821, 'mechanical' ) ;
#14691 = CARTESIAN_POINT ( 'NONE',  ( -3.219147294324499420, 2.743867526398026779, -0.6706657213163130793 ) ) ;
#14692 = CIRCLE ( 'NONE', #9984, 14.80000000000025651 ) ;
#14693 = CARTESIAN_POINT ( 'NONE',  ( -8.661991262811106651, 9.999999999999998224, -130.6821289911104316 ) ) ;
#14694 = ORIENTED_EDGE ( 'NONE', *, *, #14293, .T. ) ;
#14695 = CARTESIAN_POINT ( 'NONE',  ( 1.346194077712560944, 7.937500000000000000, -0.2500000000000011102 ) ) ;
#14696 = DIRECTION ( 'NONE',  ( -0.000000000000000000, 1.000000000000000000, -0.000000000000000000 ) ) ;
#14697 = CARTESIAN_POINT ( 'NONE',  ( 1.346194077712561166, 3.437500000000000444, -0.2500000000000011102 ) ) ;
#14698 = CARTESIAN_POINT ( 'NONE',  ( 2.298097038856278029, 10.12500000000000000, -5.798097038856279362 ) ) ;
#14699 = EDGE_CURVE ( 'NONE', #9868, #7762, #10874, .T. ) ;
#14700 = CARTESIAN_POINT ( 'NONE',  ( -1.313187589810638434, 10.00000000000000000, -105.6642581345501668 ) ) ;
#14701 = CARTESIAN_POINT ( 'NONE',  ( 10.26465888295316020, 14.41280555647187889, -106.6644705394424619 ) ) ;
#14702 = ADVANCED_FACE ( 'NONE', ( #12109 ), #10710, .F. ) ;
#14703 = CARTESIAN_POINT ( 'NONE',  ( 3.249999999999998668, 6.687500000000000888, -4.846194077712560500 ) ) ;
#14704 = AXIS2_PLACEMENT_3D ( 'NONE', #8577, #10747, #10902 ) ;
#14705 = CARTESIAN_POINT ( 'NONE',  ( -3.749999999999999556, 5.750000000000000000, -3.499999999999999112 ) ) ;
#14706 = CARTESIAN_POINT ( 'NONE',  ( 3.749999999999999556, 10.81250000000000178, -1.946699141100892261 ) ) ;
#14707 = CARTESIAN_POINT ( 'NONE',  ( -3.486358512013132849, 2.569799602646718917, -1.000000000000001110 ) ) ;
#14708 = CARTESIAN_POINT ( 'NONE',  ( 37.88191578704505957, 0.000000000000000000, 42.20832867525968624 ) ) ;
#14709 = CARTESIAN_POINT ( 'NONE',  ( 0.000000000000000000, 9.500000000000000000, 0.2500000000000002220 ) ) ;
#14710 = CARTESIAN_POINT ( 'NONE',  ( 3.906635893048721275, 14.90393432339122093, -1.513038254126030990 ) ) ;
#14711 = CARTESIAN_POINT ( 'NONE',  ( 12.62779646475434703, 2.635826865785323214, -166.1237625897486794 ) ) ;
#14712 = CIRCLE ( 'NONE', #8018, 3.500000000000003109 ) ;
#14713 = CARTESIAN_POINT ( 'NONE',  ( 8.665381006182327539, 0.6447310902546593558, -106.0007322442988738 ) ) ;
#14714 = CARTESIAN_POINT ( 'NONE',  ( -30.17254888771753585, 3.999999999999511502, -186.2931491953524983 ) ) ;
#14715 = DIRECTION ( 'NONE',  ( 0.000000000000000000, 0.000000000000000000, -1.000000000000000000 ) ) ;
#14716 = DESIGN_CONTEXT ( 'detailed design', #7479, 'design' ) ;
#14717 = CARTESIAN_POINT ( 'NONE',  ( -35.54172072645641833, 9.999999999999998224, -156.2450653135776975 ) ) ;
#14718 = CARTESIAN_POINT ( 'NONE',  ( -3.749999999999999556, 12.74999999999999822, -3.499999999999999112 ) ) ;
#14719 = ORIENTED_EDGE ( 'NONE', *, *, #12555, .T. ) ;
#14720 = DIRECTION ( 'NONE',  ( 0.000000000000000000, 0.000000000000000000, 1.000000000000000000 ) ) ;
#14721 = CARTESIAN_POINT ( 'NONE',  ( -0.3766621274091715987, 0.2004420829692335482, 0.1491815183709511161 ) ) ;
#14722 = CARTESIAN_POINT ( 'NONE',  ( -3.749999999999999556, 11.31249999999999822, -5.053300858899104853 ) ) ;
#14723 = CARTESIAN_POINT ( 'NONE',  ( 2.651650429449552870, 9.125000000000001776, -6.151650429449553314 ) ) ;
#14724 = CARTESIAN_POINT ( 'NONE',  ( 10.97171279554003043, 8.773889247172311556, -44.61149169061435060 ) ) ;
#14725 = ADVANCED_FACE ( 'NONE', ( #5161 ), #4847, .T. ) ;
#14726 = CARTESIAN_POINT ( 'NONE',  ( 3.249999999999999556, 7.250000000000000000, -3.500000000000000000 ) ) ;
#14727 = ADVANCED_FACE ( 'NONE', ( #2770 ), #5008, .F. ) ;
#14728 = CARTESIAN_POINT ( 'NONE',  ( -4.592425496802573972E-16, 13.50000000000000000, -7.249999999999999112 ) ) ;
#14729 = CARTESIAN_POINT ( 'NONE',  ( 1.243260443319662123, 6.000000000000000000, -139.4020581015306846 ) ) ;
#14730 = DIRECTION ( 'NONE',  ( 0.000000000000000000, 0.000000000000000000, 1.000000000000000000 ) ) ;
#14731 = COORDINATED_UNIVERSAL_TIME_OFFSET ( 0, 0, .AHEAD. ) ;
#14732 = CARTESIAN_POINT ( 'NONE',  ( -3.249999999999999556, 12.18750000000000000, -2.153805922287440833 ) ) ;
#14733 = CARTESIAN_POINT ( 'NONE',  ( -6.119281984250459772, 2.490287375297123962, -44.38286699775954247 ) ) ;
#14734 = DIRECTION ( 'NONE',  ( 0.9997619372588932851, -0.000000000000000000, 0.02181900108494707474 ) ) ;
#14735 = CARTESIAN_POINT ( 'NONE',  ( 9.112041370329526657, 5.000000000000000888, -109.9899024349129775 ) ) ;
#14736 = DIRECTION ( 'NONE',  ( -0.000000000000000000, -1.000000000000000000, -0.000000000000000000 ) ) ;
#14737 = CARTESIAN_POINT ( 'NONE',  ( 6.049910241306247549, 9.999999999999998224, -118.3734240199295300 ) ) ;
#14738 = CC_DESIGN_PERSON_AND_ORGANIZATION_ASSIGNMENT ( #9534, #2660, ( #7654 ) ) ;
#14739 = EDGE_LOOP ( 'NONE', ( #9116, #13649, #6274, #9782 ) ) ;
#14740 = DIRECTION ( 'NONE',  ( 0.000000000000000000, 1.000000000000000000, 0.000000000000000000 ) ) ;
#14741 = CARTESIAN_POINT ( 'NONE',  ( 10.08988835584683308, 12.49999999999999822, -120.5979435464156211 ) ) ;
#14742 = CARTESIAN_POINT ( 'NONE',  ( 0.000000000000000000, 11.50000000000000000, 0.2499999999999998057 ) ) ;
#14743 = CARTESIAN_POINT ( 'NONE',  ( 3.249999999999999556, 12.25000000000000000, -3.500000000000000000 ) ) ;
#14744 = CARTESIAN_POINT ( 'NONE',  ( 2.298097038856279362, 13.37500000000000000, -1.201902961143720860 ) ) ;
#14745 = VERTEX_POINT ( 'NONE', #12191 ) ;
#14746 = EDGE_CURVE ( 'NONE', #6908, #7480, #7237, .T. ) ;
#14747 = CARTESIAN_POINT ( 'NONE',  ( -2.298097038856278473, 11.12500000000000000, -1.201902961143720416 ) ) ;
#14748 = ADVANCED_FACE ( 'NONE', ( #14610, #4921 ), #8474, .T. ) ;
#14749 = EDGE_CURVE ( 'NONE', #7422, #7451, #1609, .T. ) ;
#14750 = CARTESIAN_POINT ( 'NONE',  ( -3.573755135672850081, -2.540697700116522739, -1.000000000000004663 ) ) ;
#14751 = CARTESIAN_POINT ( 'NONE',  ( 0.000000000000000000, 4.000000000000000000, 0.000000000000000000 ) ) ;
#14752 = CARTESIAN_POINT ( 'NONE',  ( 30.32986759126112730, 1.750000000000000000, 43.04214087805580391 ) ) ;
#14753 = CARTESIAN_POINT ( 'NONE',  ( -5.561182064723690921, 14.89159520570006379, -117.2542806587632214 ) ) ;
#14754 = APPROVAL_STATUS ( 'not_yet_approved' ) ;
#14755 = CARTESIAN_POINT ( 'NONE',  ( 13.03594997074850959, 15.00000000000000000, -125.1067209764227073 ) ) ;
#14756 = VERTEX_POINT ( 'NONE', #5086 ) ;
#14757 = CARTESIAN_POINT ( 'NONE',  ( 3.249999999999998668, 5.687500000000000000, -4.846194077712560500 ) ) ;
#14758 =( BOUNDED_CURVE ( )  B_SPLINE_CURVE ( 2, ( #13839, #4483, #1868, #7954, #3321, #9191, #930, #8031, #5632, #10052, #5338, #14791, #13623, #3024, #7731, #6573, #11285, #7019, #7083, #2463, #70, #8402, #9422, #10656, #13051, #1220, #14146, #3548, #14067, #11804, #145, #8255, #5711, #9345, #2238, #5930, #4782, #15314, #2387, #15167, #10508, #8103, #3469, #9566, #4855, #5856, #14292, #2319, #10430, #10731, #9496, #14221, #3622, #7160, #4562, #3693, #11732, #8325, #11882, #1304, #6007, #4709, #11583, #9271, #8180, #2167, #1153, #6869, #1001, #13995, #12982, #3393, #12828, #6946, #4634, #11662, #1081, #5787, #15242, #12906, #10575, #11959, #6250, #4096, #5094, #10802, #7322, #5248, #2697, #385, #8637, #3778, #8558, #1616, #6163, #9807, #7246, #2544, #12035, #13293, #4931, #1687, #10883, #1456, #7396, #9881, #3860, #303, #13134, #13373, #14538, #10967, #6398, #8486, #6328, #1383, #533, #1536, #12119, #3935, #5016, #12277, #2778, #9956, #9735, #7482, #12200, #14695, #11112, #6085, #11043, #14619, #13217, #459, #216, #5169, #4017, #8718, #13454, #2858, #7558, #9648, #2619, #14380, #14464, #8070, #5321, #4527, #6768, #13529, #616, #12720, #11191, #10397, #11481, #13888, #2282, #15053, #8799, #2927, #15279, #5753, #6988, #7631, #12347, #15208, #1765, #12793, #5823, #10546, #9309, #14033, #2131, #12642, #6475, #6834, #10034, #10314, #7922, #4375, #11550, #3205, #9160, #14771, #2056, #3429, #2200, #899, #8141, #9084, #966, #5600, #9236, #3284, #11627, #13805, #4447, #4601, #12870, #11704, #7999, #5673, #15132, #13964, #3359, #6907, #1122, #1045, #10475, #10930, #11844, #14111, #1269, #5974, #14265, #7365, #9695, #1191, #10615, #4671, #14340, #6053, #3664, #7288, #7055, #3825, #3513, #37, #13181, #8220, #7206, #1504, #189, #10697, #8448, #13023, #8526, #6215, #8365, #113, #14190 ),
 .UNSPECIFIED., .F., .F. ) 
 B_SPLINE_CURVE_WITH_KNOTS ( ( 3, 2, 2, 2, 2, 2, 2, 2, 2, 2, 2, 2, 2, 2, 2, 2, 2, 2, 2, 2, 2, 2, 2, 2, 2, 2, 2, 2, 2, 2, 2, 2, 2, 2, 2, 2, 2, 2, 2, 2, 2, 2, 2, 2, 2, 2, 2, 2, 2, 2, 2, 2, 2, 2, 2, 2, 2, 2, 2, 2, 2, 2, 2, 2, 2, 2, 2, 2, 2, 2, 2, 2, 2, 2, 2, 2, 2, 2, 2, 2, 2, 2, 2, 2, 2, 2, 2, 2, 2, 2, 2, 2, 2, 2, 2, 2, 2, 2, 2, 2, 2, 2, 2, 2, 2, 2, 2, 2, 2, 2, 2, 2, 2, 2, 2, 2, 2, 2, 2, 2, 3 ),
 ( 0.000000000000000000, 0.008333333333333333218, 0.01666666666666666644, 0.02500000000000000139, 0.03333333333333333287, 0.04166666666666666435, 0.05000000000000000278, 0.05833333333333333426, 0.06666666666666666574, 0.07499999999999999722, 0.08333333333333332871, 0.09166666666666666019, 0.1000000000000000056, 0.1083333333333333370, 0.1166666666666666685, 0.1250000000000000000, 0.1333333333333333315, 0.1416666666666666630, 0.1499999999999999944, 0.1583333333333333259, 0.1666666666666666574, 0.1749999999999999889, 0.1833333333333333204, 0.1916666666666666519, 0.2000000000000000111, 0.2083333333333333426, 0.2166666666666666741, 0.2250000000000000056, 0.2333333333333333370, 0.2416666666666666685, 0.2500000000000000000, 0.2583333333333333037, 0.2666666666666666630, 0.2750000000000000222, 0.2833333333333333259, 0.2916666666666666852, 0.2999999999999999889, 0.3083333333333333481, 0.3166666666666666519, 0.3250000000000000111, 0.3333333333333333148, 0.3416666666666666741, 0.3499999999999999778, 0.3583333333333333370, 0.3666666666666666408, 0.3750000000000000000, 0.3833333333333333037, 0.3916666666666666630, 0.4000000000000000222, 0.4083333333333333259, 0.4166666666666666852, 0.4249999999999999889, 0.4333333333333333481, 0.4416666666666666519, 0.4500000000000000111, 0.4583333333333333148, 0.4666666666666666741, 0.4749999999999999778, 0.4833333333333333370, 0.4916666666666666408, 0.5000000000000000000, 0.5083333333333333037, 0.5166666666666666075, 0.5250000000000000222, 0.5333333333333333259, 0.5416666666666666297, 0.5500000000000000444, 0.5583333333333333481, 0.5666666666666666519, 0.5749999999999999556, 0.5833333333333333703, 0.5916666666666666741, 0.5999999999999999778, 0.6083333333333332815, 0.6166666666666666963, 0.6250000000000000000, 0.6333333333333333037, 0.6416666666666666075, 0.6500000000000000222, 0.6583333333333333259, 0.6666666666666666297, 0.6750000000000000444, 0.6833333333333333481, 0.6916666666666666519, 0.6999999999999999556, 0.7083333333333333703, 0.7166666666666666741, 0.7249999999999999778, 0.7333333333333332815, 0.7416666666666666963, 0.7500000000000000000, 0.7583333333333333037, 0.7666666666666666075, 0.7750000000000000222, 0.7833333333333333259, 0.7916666666666666297, 0.8000000000000000444, 0.8083333333333333481, 0.8166666666666666519, 0.8249999999999999556, 0.8333333333333333703, 0.8416666666666666741, 0.8499999999999999778, 0.8583333333333332815, 0.8666666666666666963, 0.8750000000000000000, 0.8833333333333333037, 0.8916666666666666075, 0.9000000000000000222, 0.9083333333333333259, 0.9166666666666666297, 0.9249999999999999334, 0.9333333333333333481, 0.9416666666666666519, 0.9499999999999999556, 0.9583333333333333703, 0.9666666666666666741, 0.9749999999999999778, 0.9833333333333332815, 0.9916666666666666963, 1.000000000000000000 ),
 .UNSPECIFIED. ) 
 CURVE ( )  GEOMETRIC_REPRESENTATION_ITEM ( )  RATIONAL_B_SPLINE_CURVE ( ( 1.000000000000000000, 0.9238795325112867385, 1.000000000000000000, 0.9238795325112867385, 1.000000000000000000, 0.9238795325112867385, 1.000000000000000000, 0.9238795325112867385, 1.000000000000000000, 0.9238795325112867385, 1.000000000000000000, 0.9238795325112867385, 1.000000000000000000, 0.9238795325112867385, 1.000000000000000000, 0.9238795325112867385, 1.000000000000000000, 0.9238795325112867385, 1.000000000000000000, 0.9238795325112867385, 1.000000000000000000, 0.9238795325112867385, 1.000000000000000000, 0.9238795325112867385, 1.000000000000000000, 0.9238795325112867385, 1.000000000000000000, 0.9238795325112867385, 1.000000000000000000, 0.9238795325112867385, 1.000000000000000000, 0.9238795325112867385, 1.000000000000000000, 0.9238795325112867385, 1.000000000000000000, 0.9238795325112867385, 1.000000000000000000, 0.9238795325112867385, 1.000000000000000000, 0.9238795325112867385, 1.000000000000000000, 0.9238795325112867385, 1.000000000000000000, 0.9238795325112867385, 1.000000000000000000, 0.9238795325112867385, 1.000000000000000000, 0.9238795325112867385, 1.000000000000000000, 0.9238795325112867385, 1.000000000000000000, 0.9238795325112867385, 1.000000000000000000, 0.9238795325112867385, 1.000000000000000000, 0.9238795325112867385, 1.000000000000000000, 0.9238795325112867385, 1.000000000000000000, 0.9238795325112867385, 1.000000000000000000, 0.9238795325112867385, 1.000000000000000000, 0.9238795325112867385, 1.000000000000000000, 0.9238795325112867385, 1.000000000000000000, 0.9238795325112867385, 1.000000000000000000, 0.9238795325112867385, 1.000000000000000000, 0.9238795325112867385, 1.000000000000000000, 0.9238795325112867385, 1.000000000000000000, 0.9238795325112867385, 1.000000000000000000, 0.9238795325112867385, 1.000000000000000000, 0.9238795325112867385, 1.000000000000000000, 0.9238795325112867385, 1.000000000000000000, 0.9238795325112867385, 1.000000000000000000, 0.9238795325112867385, 1.000000000000000000, 0.9238795325112867385, 1.000000000000000000, 0.9238795325112867385, 1.000000000000000000, 0.9238795325112867385, 1.000000000000000000, 0.9238795325112867385, 1.000000000000000000, 0.9238795325112867385, 1.000000000000000000, 0.9238795325112867385, 1.000000000000000000, 0.9238795325112867385, 1.000000000000000000, 0.9238795325112867385, 1.000000000000000000, 0.9238795325112867385, 1.000000000000000000, 0.9238795325112867385, 1.000000000000000000, 0.9238795325112867385, 1.000000000000000000, 0.9238795325112867385, 1.000000000000000000, 0.9238795325112867385, 1.000000000000000000, 0.9238795325112867385, 1.000000000000000000, 0.9238795325112867385, 1.000000000000000000, 0.9238795325112867385, 1.000000000000000000, 0.9238795325112867385, 1.000000000000000000, 0.9238795325112867385, 1.000000000000000000, 0.9238795325112867385, 1.000000000000000000, 0.9238795325112867385, 1.000000000000000000, 0.9238795325112867385, 1.000000000000000000, 0.9238795325112867385, 1.000000000000000000, 0.9238795325112867385, 1.000000000000000000, 0.9238795325112867385, 1.000000000000000000, 0.9238795325112867385, 1.000000000000000000, 0.9238795325112867385, 1.000000000000000000, 0.9238795325112867385, 1.000000000000000000, 0.9238795325112867385, 1.000000000000000000, 0.9238795325112867385, 1.000000000000000000, 0.9238795325112867385, 1.000000000000000000, 0.9238795325112867385, 1.000000000000000000, 0.9238795325112867385, 1.000000000000000000, 0.9238795325112867385, 1.000000000000000000, 0.9238795325112867385, 1.000000000000000000, 0.9238795325112867385, 1.000000000000000000, 0.9238795325112867385, 1.000000000000000000, 0.9238795325112867385, 1.000000000000000000, 0.9238795325112867385, 1.000000000000000000, 0.9238795325112867385, 1.000000000000000000, 0.9238795325112867385, 1.000000000000000000, 0.9238795325112867385, 1.000000000000000000, 0.9238795325112867385, 1.000000000000000000, 0.9238795325112867385, 1.000000000000000000, 0.9238795325112867385, 1.000000000000000000, 0.9238795325112867385, 1.000000000000000000, 0.9238795325112867385, 1.000000000000000000, 0.9238795325112867385, 1.000000000000000000, 0.9238795325112867385, 1.000000000000000000, 0.9238795325112867385, 1.000000000000000000, 0.9238795325112867385, 1.000000000000000000, 0.9238795325112867385, 1.000000000000000000, 0.9238795325112867385, 1.000000000000000000, 0.9238795325112867385, 1.000000000000000000, 0.9238795325112867385, 1.000000000000000000, 0.9238795325112867385, 1.000000000000000000, 0.9238795325112867385, 1.000000000000000000, 0.9238795325112867385, 1.000000000000000000, 0.9238795325112867385, 1.000000000000000000, 0.9238795325112867385, 1.000000000000000000, 0.9238795325112867385, 1.000000000000000000, 0.9238795325112867385, 1.000000000000000000, 0.9238795325112867385, 1.000000000000000000, 0.9238795325112867385, 1.000000000000000000, 0.9238795325112867385, 1.000000000000000000, 0.9238795325112867385, 1.000000000000000000, 0.9238795325112867385, 1.000000000000000000, 0.9238795325112867385, 1.000000000000000000, 0.9238795325112867385, 1.000000000000000000, 0.9238795325112867385, 1.000000000000000000, 0.9238795325112867385, 1.000000000000000000, 0.9238795325112867385, 1.000000000000000000, 0.9238795325112867385, 1.000000000000000000, 0.9238795325112867385, 1.000000000000000000, 0.9238795325112867385, 1.000000000000000000, 0.9238795325112867385, 1.000000000000000000, 0.9238795325112867385, 1.000000000000000000, 0.9238795325112867385, 1.000000000000000000 ) ) 
 REPRESENTATION_ITEM ( '' )  );
#14759 = CARTESIAN_POINT ( 'NONE',  ( 3.749999999999999112, 11.81249999999999822, -1.946699141100892039 ) ) ;
#14760 = ORIENTED_EDGE ( 'NONE', *, *, #11504, .T. ) ;
#14761 = CARTESIAN_POINT ( 'NONE',  ( 5.844703153020811115, 5.000000000000000888, -103.2023327213425432 ) ) ;
#14762 = CARTESIAN_POINT ( 'NONE',  ( 0.000000000000000000, 15.50000000000000178, 0.2499999999999998057 ) ) ;
#14763 = CC_DESIGN_DATE_AND_TIME_ASSIGNMENT ( #9642, #3930, ( #1046 ) ) ;
#14764 = CARTESIAN_POINT ( 'NONE',  ( 7.265156645817275383, 3.132533400630292952, -23.06457822180372119 ) ) ;
#14765 = CARTESIAN_POINT ( 'NONE',  ( 3.200329101915443175, 3.382469978819814038, 4.943050645478439087 ) ) ;
#14766 = AXIS2_PLACEMENT_3D ( 'NONE', #3819, #1574, #9687 ) ;
#14767 = CARTESIAN_POINT ( 'NONE',  ( 11.28440626344662157, 4.315957715789585869, -106.3983886562123331 ) ) ;
#14768 = PERSON_AND_ORGANIZATION_ROLE ( 'classification_officer' ) ;
#14769 = DIRECTION ( 'NONE',  ( 0.000000000000000000, 1.000000000000000000, 0.000000000000000000 ) ) ;
#14770 = ORIENTED_EDGE ( 'NONE', *, *, #5327, .T. ) ;
#14771 = CARTESIAN_POINT ( 'NONE',  ( -1.346194077712559167, 11.43750000000000000, -6.749999999999999112 ) ) ;
#14772 = DIRECTION ( 'NONE',  ( 0.7575874476598360996, -0.000000000000000000, 0.6527336816407247611 ) ) ;
#14773 = CARTESIAN_POINT ( 'NONE',  ( -3.249999999999999112, 1.812499999999999778, -4.846194077712558723 ) ) ;
#14774 = CARTESIAN_POINT ( 'NONE',  ( 1.346194077712561166, 9.437500000000000000, -0.2500000000000011102 ) ) ;
#14775 = CARTESIAN_POINT ( 'NONE',  ( -0.2500000000000000555, 4.500000000000000888, -1.499999999999999778 ) ) ;
#14776 = FACE_OUTER_BOUND ( 'NONE', #1866, .T. ) ;
#14777 = CARTESIAN_POINT ( 'NONE',  ( -1.346194077712559389, 5.437500000000002665, -6.749999999999999112 ) ) ;
#14778 = CARTESIAN_POINT ( 'NONE',  ( 2.651650429449552870, 5.125000000000000000, -6.151650429449553314 ) ) ;
#14779 = CARTESIAN_POINT ( 'NONE',  ( -1.553300858899106407, 8.062500000000000000, 0.2500000000000002220 ) ) ;
#14780 = FACE_OUTER_BOUND ( 'NONE', #8275, .T. ) ;
#14781 = EDGE_LOOP ( 'NONE', ( #3341, #13820, #3397, #4445 ) ) ;
#14782 = CARTESIAN_POINT ( 'NONE',  ( -3.315923205871639468, 9.650666666666662508, -43.24506100211545601 ) ) ;
#14783 = CARTESIAN_POINT ( 'NONE',  ( -2.651650429449553314, 11.87500000000000000, -6.151650429449552426 ) ) ;
#14784 = CARTESIAN_POINT ( 'NONE',  ( 3.882360952064769943, 14.89515687073112460, -1.256691955966320329 ) ) ;
#14785 = CARTESIAN_POINT ( 'NONE',  ( 9.920343557553863434, 0.09491738922561235303, -163.9751099406502703 ) ) ;
#14786 = B_SPLINE_CURVE_WITH_KNOTS ( 'NONE', 3,
 ( #13069, #3571, #8198, #7179, #8273, #9288, #3410, #4650, #1326, #13001, #12928, #6029, #1245, #14088, #5951, #9211, #4804, #3491, #9518, #13942 ),
 .UNSPECIFIED., .F., .F.,
 ( 4, 2, 2, 2, 2, 2, 2, 2, 2, 4 ),
 ( -1.586017202738188953E-05, 0.001008001390798507393, 0.002031862953624396628, 0.003055724516450285862, 0.004079586079276174664, 0.005103447642102064766, 0.005615378423515009383, 0.006127309204927953133, 0.007151170767753843235, 0.008175032330579735940 ),
 .UNSPECIFIED. ) ;
#14787 = EDGE_CURVE ( 'NONE', #13724, #4391, #3683, .T. ) ;
#14788 = EDGE_CURVE ( 'NONE', #5990, #4897, #4480, .T. ) ;
#14789 = CARTESIAN_POINT ( 'NONE',  ( -8.205916711996726676, 7.499999999999991118, -92.94857034792688921 ) ) ;
#14790 = CARTESIAN_POINT ( 'NONE',  ( -24.49765103532420341, 5.421660010089610387E-13, -170.6954199489630355 ) ) ;
#14791 = CARTESIAN_POINT ( 'NONE',  ( 3.249999999999998668, 0.6875000000000000000, -4.846194077712560500 ) ) ;
#14792 = CARTESIAN_POINT ( 'NONE',  ( -41.27834176925853882, 14.99999999999932676, -157.9203444101418938 ) ) ;
#14793 = CARTESIAN_POINT ( 'NONE',  ( -1.553300858899106629, 13.56250000000000000, 0.2500000000000002220 ) ) ;
#14794 = ORIENTED_EDGE ( 'NONE', *, *, #11695, .F. ) ;
#14795 = CARTESIAN_POINT ( 'NONE',  ( 10.94278504614969982, 5.000000000000001776, -43.28600191872154568 ) ) ;
#14796 = CARTESIAN_POINT ( 'NONE',  ( 9.573673229721526567, 1.209833687612193343, -105.8952646585356234 ) ) ;
#14797 = CARTESIAN_POINT ( 'NONE',  ( 1.553300858899109071, 10.43750000000000178, 0.2499999999999989175 ) ) ;
#14798 = CARTESIAN_POINT ( 'NONE',  ( -3.329342754288864281, 9.806926398386266897, -43.39706447520367050 ) ) ;
#14799 = CARTESIAN_POINT ( 'NONE',  ( -9.076832803613504197, 2.617545850183311540, -116.5147594324866134 ) ) ;
#14800 = CARTESIAN_POINT ( 'NONE',  ( -3.249999999999999556, 8.750000000000001776, -3.500000000000000000 ) ) ;
#14801 = CARTESIAN_POINT ( 'NONE',  ( 6.422699671861705539, 4.000000000000000000, -139.1645012375703061 ) ) ;
#14802 = CARTESIAN_POINT ( 'NONE',  ( 2.651650429449552870, 12.62500000000000000, -6.151650429449554203 ) ) ;
#14803 = DIRECTION ( 'NONE',  ( 0.000000000000000000, -1.000000000000000000, 0.000000000000000000 ) ) ;
#14804 = CARTESIAN_POINT ( 'NONE',  ( 1.831246893856141034, 2.490287375297123518, -1.000000000000028644 ) ) ;
#14805 = CARTESIAN_POINT ( 'NONE',  ( 3.249999999999998668, 10.68750000000000000, -4.846194077712560500 ) ) ;
#14806 = LINE ( 'NONE', #4132, #8062 ) ;
#14807 = EDGE_CURVE ( 'NONE', #14600, #7347, #12637, .T. ) ;
#14808 = CYLINDRICAL_SURFACE ( 'NONE', #5056, 3.500000000000003109 ) ;
#14809 = CARTESIAN_POINT ( 'NONE',  ( 3.473492316508982380, 8.673617379884035472E-16, -116.2542051831695602 ) ) ;
#14810 = DIRECTION ( 'NONE',  ( 0.08794243244722413366, 0.000000000000000000, 0.9961255586397056438 ) ) ;
#14811 = CARTESIAN_POINT ( 'NONE',  ( -63.21422130130007133, 9.999999999999998224, -203.6040552426024703 ) ) ;
#14812 = ORIENTED_EDGE ( 'NONE', *, *, #4515, .F. ) ;
#14813 = CARTESIAN_POINT ( 'NONE',  ( 8.973057892629592303, 12.37556808675488718, 1.136665787335843669 ) ) ;
#14814 = CARTESIAN_POINT ( 'NONE',  ( 9.348010916527714542, 12.50000000000000000, -118.9691738015868339 ) ) ;
#14815 = CARTESIAN_POINT ( 'NONE',  ( 0.000000000000000000, 15.50000000000000178, 0.2499999999999998057 ) ) ;
#14816 = CARTESIAN_POINT ( 'NONE',  ( -2.298097038856279362, 9.875000000000000000, -5.798097038856278473 ) ) ;
#14817 = CARTESIAN_POINT ( 'NONE',  ( 0.000000000000000000, 1.000000000000000000, -0.2500000000000002220 ) ) ;
#14818 = ORIENTED_EDGE ( 'NONE', *, *, #14043, .T. ) ;
#14819 = CARTESIAN_POINT ( 'NONE',  ( 3.249999999999999556, 10.75000000000000000, -3.500000000000000000 ) ) ;
#14820 = CARTESIAN_POINT ( 'NONE',  ( 10.98449899626661974, 11.68766481771978505, -45.34906724785665233 ) ) ;
#14821 = CARTESIAN_POINT ( 'NONE',  ( -4.090890948359604984, 15.00000000000000000, -103.1929727064838147 ) ) ;
#14822 = CARTESIAN_POINT ( 'NONE',  ( -25.06471962037405277, 4.000000000000000000, -209.2255395231934472 ) ) ;
#14823 = DIRECTION ( 'NONE',  ( 0.1564344650402314796, 0.000000000000000000, 0.9876883405951375483 ) ) ;
#14824 = ITEM_DEFINED_TRANSFORMATION ( 'NONE', 'NONE', #9179,  #9419 ) ;
#14825 = CARTESIAN_POINT ( 'NONE',  ( 9.136110106353408256, 12.49999999999999822, -109.8557328641390711 ) ) ;
#14826 = EDGE_CURVE ( 'NONE', #119, #12332, #5962, .T. ) ;
#14827 = CARTESIAN_POINT ( 'NONE',  ( 23.30137936743921756, 0.3998921152664920986, -138.6870304616822693 ) ) ;
#14828 = EDGE_CURVE ( 'NONE', #8798, #1605, #11791, .T. ) ;
#14829 = ORIENTED_EDGE ( 'NONE', *, *, #13682, .F. ) ;
#14830 = CARTESIAN_POINT ( 'NONE',  ( 3.249999999999999556, 3.750000000000000000, -3.500000000000000000 ) ) ;
#14831 = CARTESIAN_POINT ( 'NONE',  ( 1.167531179896771798, 4.000000000000000000, -139.4941991647475845 ) ) ;
#14832 = CARTESIAN_POINT ( 'NONE',  ( 1.553300858899105963, 3.062500000000000000, -7.250000000000000888 ) ) ;
#14833 = ORIENTED_EDGE ( 'NONE', *, *, #12833, .F. ) ;
#14834 = LOCAL_TIME ( 12, 28, 20.00000000000000000, #11941 ) ;
#14835 = DIRECTION ( 'NONE',  ( 0.9997619372588932851, 0.000000000000000000, 0.02181900108494707821 ) ) ;
#14836 = VECTOR ( 'NONE', #2196, 1000.000000000000000 ) ;
#14837 = CARTESIAN_POINT ( 'NONE',  ( -1.553300858899107295, 3.437500000000000000, -7.250000000000000000 ) ) ;
#14838 = CARTESIAN_POINT ( 'NONE',  ( 7.492004171561701398, 3.557029191498670695, -21.78040058436872428 ) ) ;
#14839 = CARTESIAN_POINT ( 'NONE',  ( 0.06906476797019409086, 2.515634231730215831, 0.7822979040126908368 ) ) ;
#14840 = CARTESIAN_POINT ( 'NONE',  ( -3.750000000000000000, 1.312500000000000222, -5.053300858899105741 ) ) ;
#14841 = PERSON_AND_ORGANIZATION ( #3176, #3020 ) ;
#14842 = APPROVAL_PERSON_ORGANIZATION ( #9606, #9706, #183 ) ;
#14843 = CARTESIAN_POINT ( 'NONE',  ( 8.328184646254079837, 5.000000000000001776, -113.2132428591397542 ) ) ;
#14844 = PLANE ( 'NONE',  #13849 ) ;
#14845 = CIRCLE ( 'NONE', #10608, 5.000000000000000000 ) ;
#14846 = ADVANCED_FACE ( 'NONE', ( #14455 ), #8623, .T. ) ;
#14847 = ORIENTED_EDGE ( 'NONE', *, *, #6940, .T. ) ;
#14848 = LINE ( 'NONE', #8800, #12613 ) ;
#14849 = CARTESIAN_POINT ( 'NONE',  ( -1.346194077712559167, 1.937500000000000222, -6.749999999999999112 ) ) ;
#14850 = CARTESIAN_POINT ( 'NONE',  ( -3.980102097228897738E-16, 13.00000000000000000, -6.749999999999999112 ) ) ;
#14851 = CARTESIAN_POINT ( 'NONE',  ( -8.226857985479757218, 10.00000000000000000, -114.4011953629546241 ) ) ;
#14852 = CIRCLE ( 'NONE', #8159, 6.999999999999950262 ) ;
#14853 = CARTESIAN_POINT ( 'NONE',  ( 11.04730217088352617, 12.49999999999999822, -107.1178495010082088 ) ) ;
#14854 = AXIS2_PLACEMENT_3D ( 'NONE', #14481, #8816, #13545 ) ;
#14855 = CARTESIAN_POINT ( 'NONE',  ( -3.749999999999999556, 3.750000000000000444, -3.499999999999999112 ) ) ;
#14856 = VECTOR ( 'NONE', #7001, 1000.000000000000000 ) ;
#14857 = CARTESIAN_POINT ( 'NONE',  ( -4.592425496802573972E-16, 8.500000000000000000, -7.249999999999999112 ) ) ;
#14858 = LINE ( 'NONE', #11128, #4232 ) ;
#14859 = ORIENTED_EDGE ( 'NONE', *, *, #935, .F. ) ;
#14860 = CARTESIAN_POINT ( 'NONE',  ( 0.4616602863826355096, 0.000000000000000000, -0.1920150514337515824 ) ) ;
#14861 = CARTESIAN_POINT ( 'NONE',  ( -1.553300858899106629, 8.562500000000000000, 0.2500000000000002220 ) ) ;
#14862 = CARTESIAN_POINT ( 'NONE',  ( 4.999922786458842694, 0.03165940129594203845, -16.23938796091260528 ) ) ;
#14863 = CARTESIAN_POINT ( 'NONE',  ( 5.904219792619186613, 15.00000000000000000, -112.3087459549632428 ) ) ;
#14864 = CARTESIAN_POINT ( 'NONE',  ( 4.950900406836915124, 5.000000000000000888, -134.4284351762048573 ) ) ;
#14865 = VECTOR ( 'NONE', #5482, 1000.000000000000000 ) ;
#14866 = EDGE_LOOP ( 'NONE', ( #11928, #3187, #8589, #3206 ) ) ;
#14867 = CARTESIAN_POINT ( 'NONE',  ( -23.99665711257156886, 8.673617379884035472E-16, -181.0464554320757884 ) ) ;
#14868 = CARTESIAN_POINT ( 'NONE',  ( 12.66298273264138174, 3.439231053088831036, -166.5121423616285767 ) ) ;
#14869 = CARTESIAN_POINT ( 'NONE',  ( -40.71937926017810838, 9.999999999999998224, -157.6611590844387365 ) ) ;
#14870 = CARTESIAN_POINT ( 'NONE',  ( 2.651650429449554203, 12.37500000000000178, -0.8483495705504471296 ) ) ;
#14871 = ORIENTED_EDGE ( 'NONE', *, *, #7532, .T. ) ;
#14872 = LINE ( 'NONE', #5342, #14440 ) ;
#14873 = CARTESIAN_POINT ( 'NONE',  ( -18.09353981420494151, 5.000000000000000000, -129.3374956033359240 ) ) ;
#14874 = FACE_OUTER_BOUND ( 'NONE', #1904, .T. ) ;
#14875 = CARTESIAN_POINT ( 'NONE',  ( -5.318033920858916908, 9.999999999999998224, -111.4753907371908923 ) ) ;
#14876 = CARTESIAN_POINT ( 'NONE',  ( -1.346194077712558945, 9.562500000000000000, -0.2500000000000002220 ) ) ;
#14877 = FACE_OUTER_BOUND ( 'NONE', #2317, .T. ) ;
#14878 = CARTESIAN_POINT ( 'NONE',  ( 1.553300858899108849, 11.93750000000000000, 0.2499999999999993616 ) ) ;
#14879 = FACE_OUTER_BOUND ( 'NONE', #8844, .T. ) ;
#14880 = CARTESIAN_POINT ( 'NONE',  ( 10.99551757066058322, 11.56847231179307478, -45.70224318734323532 ) ) ;
#14881 = CARTESIAN_POINT ( 'NONE',  ( 2.298097038856278473, 12.62500000000000000, -5.798097038856279362 ) ) ;
#14882 = CARTESIAN_POINT ( 'NONE',  ( 6.369258321017759350, 2.529993217055222843, -34.56909192082981974 ) ) ;
#14883 = LINE ( 'NONE', #9135, #8998 ) ;
#14884 = CARTESIAN_POINT ( 'NONE',  ( 0.000000000000000000, 9.000000000000001776, -0.2500000000000002220 ) ) ;
#14885 = DIRECTION ( 'NONE',  ( -0.9997619372588931741, -0.000000000000000000, -0.02181900108494707474 ) ) ;
#14886 = CARTESIAN_POINT ( 'NONE',  ( 1.320501113854931630, 5.000000000000000888, -137.8664870916819893 ) ) ;
#14887 = CARTESIAN_POINT ( 'NONE',  ( -3.249999999999999112, 5.687500000000000888, -2.153805922287440833 ) ) ;
#14888 = ORIENTED_EDGE ( 'NONE', *, *, #11774, .F. ) ;
#14889 = CARTESIAN_POINT ( 'NONE',  ( 0.000000000000000000, 1.530808498934191509E-17, 0.000000000000000000 ) ) ;
#14890 = CARTESIAN_POINT ( 'NONE',  ( 14.22910372453204353, 12.49999999999999822, -126.5134921567817941 ) ) ;
#14891 = CARTESIAN_POINT ( 'NONE',  ( -1.553300858899107295, 0.4375000000000000555, -7.250000000000000000 ) ) ;
#14892 = CARTESIAN_POINT ( 'NONE',  ( -2.651650429449552870, 0.6249999999999998890, -0.8483495705504467965 ) ) ;
#14893 = CARTESIAN_POINT ( 'NONE',  ( -3.249999999999999556, 1.250000000000000000, -3.499999999999999556 ) ) ;
#14894 = EDGE_CURVE ( 'NONE', #6134, #8293, #4315, .T. ) ;
#14895 = ORIENTED_EDGE ( 'NONE', *, *, #15218, .T. ) ;
#14896 = CARTESIAN_POINT ( 'NONE',  ( 1.346194077712558057, 9.562500000000000000, -6.750000000000000000 ) ) ;
#14897 = EDGE_CURVE ( 'NONE', #8964, #9805, #5931, .T. ) ;
#14898 = CARTESIAN_POINT ( 'NONE',  ( 10.94790802041948652, 11.56847231179307478, -43.52074019388547299 ) ) ;
#14899 = CARTESIAN_POINT ( 'NONE',  ( -7.072992149635495274, 2.500000000000000888, -107.3904655700100648 ) ) ;
#14900 = CARTESIAN_POINT ( 'NONE',  ( 5.456070725290617318, 2.049461655773607394, 4.191750790487847489 ) ) ;
#14901 = CARTESIAN_POINT ( 'NONE',  ( -9.721966606378854792, 10.00000000000000000, -116.3614657639809451 ) ) ;
#14902 = DATE_AND_TIME ( #1745, #2960 ) ;
#14903 = CARTESIAN_POINT ( 'NONE',  ( 12.15266112757328898, 12.49999999999999822, -123.9192486816531442 ) ) ;
#14904 = CARTESIAN_POINT ( 'NONE',  ( -9.525540565743060739, 11.37243141597640061, -116.4087343257888705 ) ) ;
#14905 = CIRCLE ( 'NONE', #7966, 2.500000000000000444 ) ;
#14906 = CARTESIAN_POINT ( 'NONE',  ( 26.30988878369277018, 2.644888176784162326, -138.3124949328119726 ) ) ;
#14907 = ORIENTED_EDGE ( 'NONE', *, *, #9281, .F. ) ;
#14908 = CARTESIAN_POINT ( 'NONE',  ( -2.298097038856278473, 5.125000000000000000, -1.201902961143720416 ) ) ;
#14909 = DIRECTION ( 'NONE',  ( 0.000000000000000000, -1.000000000000000000, 0.000000000000000000 ) ) ;
#14910 = CARTESIAN_POINT ( 'NONE',  ( -3.750000000000000000, 0.6875000000000000000, -1.946699141100893149 ) ) ;
#14911 = EDGE_LOOP ( 'NONE', ( #4159, #14513, #11667, #9494, #516, #1084, #5895, #11705, #14486, #8282 ) ) ;
#14912 = CARTESIAN_POINT ( 'NONE',  ( 29.21736815051484015, 8.773889247172311556, -44.21329492081407153 ) ) ;
#14913 = CARTESIAN_POINT ( 'NONE',  ( -0.3766621274091715987, 0.5000000000000000000, 0.1491815183709511716 ) ) ;
#14914 = ADVANCED_FACE ( 'NONE', ( #10412, #2069, #11715 ), #11495, .F. ) ;
#14915 = CARTESIAN_POINT ( 'NONE',  ( -2.651650429449553314, 5.375000000000000000, -6.151650429449552426 ) ) ;
#14916 = AXIS2_PLACEMENT_3D ( 'NONE', #13460, #9888, #3011 ) ;
#14917 = EDGE_CURVE ( 'NONE', #10346, #11885, #5767, .T. ) ;
#14918 = CARTESIAN_POINT ( 'NONE',  ( 7.442588453438189866, 4.718804654235878360, -26.16159948206511032 ) ) ;
#14919 = CARTESIAN_POINT ( 'NONE',  ( 0.1113112812214025055, 2.624162859069118170, 1.260824940869380573 ) ) ;
#14920 = CARTESIAN_POINT ( 'NONE',  ( 3.750000000000000000, 2.750000000000000000, -3.500000000000000444 ) ) ;
#14921 = APPLICATION_PROTOCOL_DEFINITION ( 'international standard', 'config_control_design', 1994, #6610 ) ;
#14922 = CARTESIAN_POINT ( 'NONE',  ( 17.88039419560352172, 5.000000000000000888, -130.2352974121733951 ) ) ;
#14923 = FACE_OUTER_BOUND ( 'NONE', #5935, .T. ) ;
#14924 = VERTEX_POINT ( 'NONE', #12735 ) ;
#14925 = CARTESIAN_POINT ( 'NONE',  ( -17.32624372123753886, 9.999999999999998224, -122.3796757791585321 ) ) ;
#14926 = AXIS2_PLACEMENT_3D ( 'NONE', #5065, #13424, #10934 ) ;
#14927 = CARTESIAN_POINT ( 'NONE',  ( 1.346194077712561166, 1.437500000000000000, -0.2500000000000011102 ) ) ;
#14928 = CARTESIAN_POINT ( 'NONE',  ( 11.03230074683944473, 12.83501270603766997, -107.1089630900316791 ) ) ;
#14929 = CARTESIAN_POINT ( 'NONE',  ( -10.71664336910952819, 4.336808689942017736E-16, -125.5340273013442527 ) ) ;
#14930 = CARTESIAN_POINT ( 'NONE',  ( 1.553300858899109071, 5.437500000000000888, 0.2499999999999989175 ) ) ;
#14931 = ADVANCED_FACE ( 'NONE', ( #8156 ), #9662, .T. ) ;
#14932 = CARTESIAN_POINT ( 'NONE',  ( 3.749999999999999112, 11.68750000000000000, -5.053300858899108405 ) ) ;
#14933 = CARTESIAN_POINT ( 'NONE',  ( 0.3766621274091715987, -0.2500000000000000000, -7.146945437571387671 ) ) ;
#14934 = ORIENTED_EDGE ( 'NONE', *, *, #6779, .T. ) ;
#14935 = CARTESIAN_POINT ( 'NONE',  ( -0.4453226528549816265, -2.225540348348185052E-17, -1.000000000000000000 ) ) ;
#14936 = CARTESIAN_POINT ( 'NONE',  ( 3.749999999999999556, 12.25000000000000000, -3.500000000000000444 ) ) ;
#14937 = CIRCLE ( 'NONE', #9730, 3.500000000000003109 ) ;
#14938 = CARTESIAN_POINT ( 'NONE',  ( -33.91109452337774854, 10.00000000000000178, -156.1716796081737471 ) ) ;
#14939 = CARTESIAN_POINT ( 'NONE',  ( 11.32016196459912649, 5.000000000000000888, -106.4092894470390291 ) ) ;
#14940 = DIRECTION ( 'NONE',  ( 0.000000000000000000, 0.000000000000000000, -1.000000000000000000 ) ) ;
#14941 = ORIENTED_EDGE ( 'NONE', *, *, #9219, .F. ) ;
#14942 = CARTESIAN_POINT ( 'NONE',  ( -29.86630916335285946, 1.632654739009349985E-12, -191.5040656882066799 ) ) ;
#14943 = CARTESIAN_POINT ( 'NONE',  ( 9.283947375375564803, 1.156835247712560688E-15, -163.3899434529763539 ) ) ;
#14944 = CARTESIAN_POINT ( 'NONE',  ( -32.01906953551642943, 15.00000000000000000, -156.2419951536765836 ) ) ;
#14945 = CARTESIAN_POINT ( 'NONE',  ( 3.249999999999998224, 4.312500000000000000, -2.153805922287439945 ) ) ;
#14946 = ORIENTED_EDGE ( 'NONE', *, *, #2909, .T. ) ;
#14947 = CARTESIAN_POINT ( 'NONE',  ( 10.32040002734025741, 5.000000000000000888, -106.4311084481271763 ) ) ;
#14948 = CARTESIAN_POINT ( 'NONE',  ( -14.68073284315481253, 7.499999999999991118, -92.37694453701993780 ) ) ;
#14949 = AXIS2_PLACEMENT_3D ( 'NONE', #15275, #9305, #2195 ) ;
#14950 = CARTESIAN_POINT ( 'NONE',  ( -25.22418021123103671, 0.005679765489689153624, -199.5580873402903421 ) ) ;
#14951 = CARTESIAN_POINT ( 'NONE',  ( 6.134629758992640625, 11.62037896290623884, 5.022017130777459926 ) ) ;
#14952 = CARTESIAN_POINT ( 'NONE',  ( 3.167496085401364958, 8.673617379884035472E-16, -107.8568673623658754 ) ) ;
#14953 = CARTESIAN_POINT ( 'NONE',  ( -2.298097038856278029, 8.625000000000000000, -1.201902961143720638 ) ) ;
#14954 = CARTESIAN_POINT ( 'NONE',  ( -1.500000000000000000, 5.000000000000000000, -0.2499999999999997780 ) ) ;
#14955 = CARTESIAN_POINT ( 'NONE',  ( -2.651650429449552870, -0.3749999999999998890, -0.8483495705504463524 ) ) ;
#14956 = CARTESIAN_POINT ( 'NONE',  ( -1.500000000000000000, 4.500000000000000888, 0.2500000000000002220 ) ) ;
#14957 = DIRECTION ( 'NONE',  ( 2.672056983927306511E-18, 1.000000000000000000, -1.224355256373460583E-16 ) ) ;
#14958 = CARTESIAN_POINT ( 'NONE',  ( 3.249999999999998668, 12.68750000000000178, -4.846194077712560500 ) ) ;
#14959 = B_SPLINE_CURVE_WITH_KNOTS ( 'NONE', 3,
 ( #4353, #13783, #3181, #12238, #9922, #14655, #1720, #574, #8832, #4202, #7671, #6516, #11231, #9133, #11599, #11679, #4423, #6743, #13860, #1096, #11455, #3336, #10522, #13937, #1021, #10293, #9285, #5648, #12772, #1167 ),
 .UNSPECIFIED., .F., .F.,
 ( 4, 2, 2, 2, 2, 2, 2, 2, 2, 2, 2, 2, 2, 2, 4 ),
 ( 5.419449386414208742E-17, 0.001566971827987180023, 0.003133943655974308004, 0.004700915483961435118, 0.005484401397954979593, 0.006267887311948524935, 0.009401830967922705437, 0.01018531688191624124, 0.01096880279590977531, 0.01253577462389684344, 0.01410274645188391504, 0.01566971827987098317, 0.01880366193584512291, 0.02193760559181925918, 0.02507154924779336769 ),
 .UNSPECIFIED. ) ;
#14960 = CYLINDRICAL_SURFACE ( 'NONE', #2641, 14.80000000000025651 ) ;
#14961 = CARTESIAN_POINT ( 'NONE',  ( 4.890948729886716251, 14.76960206134759090, 0.2075543622030249502 ) ) ;
#14962 = CARTESIAN_POINT ( 'NONE',  ( -1.346194077712559389, 10.43750000000000000, -6.749999999999999112 ) ) ;
#14963 = CARTESIAN_POINT ( 'NONE',  ( 6.089666224640342129, 0.000000000000000000, -124.6062682140657216 ) ) ;
#14964 = DIRECTION ( 'NONE',  ( 0.000000000000000000, 0.000000000000000000, 1.000000000000000000 ) ) ;
#14965 = ORIENTED_EDGE ( 'NONE', *, *, #4385, .F. ) ;
#14966 = DIRECTION ( 'NONE',  ( 0.9026204165532970558, 0.000000000000000000, 0.4304374328763154733 ) ) ;
#14967 = DIRECTION ( 'NONE',  ( 0.000000000000000000, 1.000000000000000000, 0.000000000000000000 ) ) ;
#14968 = CARTESIAN_POINT ( 'NONE',  ( 3.749999999999998668, 0.6875000000000000000, -5.053300858899107517 ) ) ;
#14969 = CARTESIAN_POINT ( 'NONE',  ( 2.298097038856279362, 14.37500000000000000, -1.201902961143720860 ) ) ;
#14970 = CARTESIAN_POINT ( 'NONE',  ( -2.298097038856278918, 1.375000000000000000, -5.798097038856277585 ) ) ;
#14971 = ORIENTED_EDGE ( 'NONE', *, *, #10056, .F. ) ;
#14972 = CARTESIAN_POINT ( 'NONE',  ( 2.298097038856278473, 9.625000000000000000, -5.798097038856279362 ) ) ;
#14973 = CARTESIAN_POINT ( 'NONE',  ( 10.96506322933161570, 11.77387500534620557, -44.79864310745833933 ) ) ;
#14974 = CARTESIAN_POINT ( 'NONE',  ( -32.22662898424438538, 15.00000000000000000, -135.0284069691736306 ) ) ;
#14975 = CARTESIAN_POINT ( 'NONE',  ( -8.456080320763300406, 13.34348931139960293, -116.2291922150413654 ) ) ;
#14976 = APPROVAL_ROLE ( '' ) ;
#14977 = CARTESIAN_POINT ( 'NONE',  ( 5.990830680408624431, 15.00000000000000000, -116.1960808033739880 ) ) ;
#14978 =( BOUNDED_SURFACE ( )  B_SPLINE_SURFACE ( 3, 1, ( 
 ( #10651, #66 ),
 ( #4775, #11877 ),
 ( #3688, #9492 ),
 ( #14215, #4851 ) ),
 .UNSPECIFIED., .F., .F., .T. ) 
 B_SPLINE_SURFACE_WITH_KNOTS ( ( 4, 4 ),
 ( 2, 2 ),
 ( 0.000000000000000000, 1.000000000000000000 ),
 ( 0.000000000000000000, 1.000000000000000000 ),
 .UNSPECIFIED. ) 
 GEOMETRIC_REPRESENTATION_ITEM ( )  RATIONAL_B_SPLINE_SURFACE ( (
 ( 1.000000000000000000, 1.000000000000000000),
 ( 0.9983030522886272573, 0.9983030522886272573),
 ( 0.9983030522886272573, 0.9983030522886272573),
 ( 1.000000000000000000, 1.000000000000000000) ) ) 
 REPRESENTATION_ITEM ( '' )  SURFACE ( )  );
#14979 = CARTESIAN_POINT ( 'NONE',  ( 24.58533183484775719, 0.8477912208884822443, -138.1065029955142620 ) ) ;
#14980 = ORIENTED_EDGE ( 'NONE', *, *, #3847, .F. ) ;
#14981 = CARTESIAN_POINT ( 'NONE',  ( -3.249999999999999556, 5.312500000000001776, -4.846194077712557835 ) ) ;
#14982 = CARTESIAN_POINT ( 'NONE',  ( -26.52423092236888635, 4.000000000000000888, -173.1808044485809717 ) ) ;
#14983 = CARTESIAN_POINT ( 'NONE',  ( 3.750000000000000000, 1.312500000000000444, -1.946699141100892705 ) ) ;
#14984 = VERTEX_POINT ( 'NONE', #4613 ) ;
#14985 = CARTESIAN_POINT ( 'NONE',  ( 11.06582261942825518, 1.749999999999318767, 58.43087504082885175 ) ) ;
#14986 = CARTESIAN_POINT ( 'NONE',  ( 7.429600267620980247, 5.211846493442712003, -26.37897252452876984 ) ) ;
#14987 = CARTESIAN_POINT ( 'NONE',  ( 3.749999999999999112, 4.812500000000000888, -1.946699141100892039 ) ) ;
#14988 = CARTESIAN_POINT ( 'NONE',  ( -25.23790167279625862, 0.7328807590307473419, -204.7435413102125210 ) ) ;
#14989 = CARTESIAN_POINT ( 'NONE',  ( 3.230086961653170885, 4.671585941591766655, 5.208283729125869677 ) ) ;
#14990 = PERSON_AND_ORGANIZATION_ROLE ( 'design_owner' ) ;
#14991 = DIRECTION ( 'NONE',  ( -0.9997619372588932851, 0.000000000000000000, -0.02181900108494707474 ) ) ;
#14992 = EDGE_LOOP ( 'NONE', ( #11684, #9501, #3427, #8427 ) ) ;
#14993 = EDGE_CURVE ( 'NONE', #9880, #2807, #12016, .T. ) ;
#14994 = CARTESIAN_POINT ( 'NONE',  ( -1.346194077712558945, 2.562500000000000444, -0.2500000000000002220 ) ) ;
#14995 = DIRECTION ( 'NONE',  ( 0.000000000000000000, 1.000000000000000000, 0.000000000000000000 ) ) ;
#14996 = PERSON ( 'NAUO-PER2', 'UNSPECIFIED', 'UNSPECIFIED', ('UNSPECIFIED'), ('UNSPECIFIED'), ('UNSPECIFIED') ) ;
#14997 = CARTESIAN_POINT ( 'NONE',  ( 2.651650429449552870, 11.12500000000000178, -6.151650429449553314 ) ) ;
#14998 = CLOSED_SHELL ( 'NONE', ( #2121, #10932, #11025, #7907, #11211, #15210, #12175, #5825, #13504, #12535, #2261, #12689, #12969, #15295, #1863, #7437, #1754 ) ) ;
#14999 = CARTESIAN_POINT ( 'NONE',  ( 1.553300858899105963, 11.56250000000000000, -7.250000000000000000 ) ) ;
#15000 = CARTESIAN_POINT ( 'NONE',  ( 3.891364641103949307, 14.90536770052033688, -1.768596708628434211 ) ) ;
#15001 = ORIENTED_EDGE ( 'NONE', *, *, #14514, .F. ) ;
#15002 = CARTESIAN_POINT ( 'NONE',  ( -6.572203743845886237, 0.4630310843464179871, -117.0568686706825048 ) ) ;
#15003 = CARTESIAN_POINT ( 'NONE',  ( -2.298097038856279362, 0.8750000000000000000, -5.798097038856278473 ) ) ;
#15004 = CARTESIAN_POINT ( 'NONE',  ( 11.32016196459912649, 12.49999999999999822, -106.4092894470390291 ) ) ;
#15005 = CARTESIAN_POINT ( 'NONE',  ( -3.979291902599172648, -10.46819190899177165, -162.6376854800281251 ) ) ;
#15006 = CARTESIAN_POINT ( 'NONE',  ( 5.228075279701640099, 4.000000000000000000, -167.7939279834373849 ) ) ;
#15007 = LINE ( 'NONE', #6722, #1729 ) ;
#15008 = ORIENTED_EDGE ( 'NONE', *, *, #1771, .T. ) ;
#15009 = EDGE_CURVE ( 'NONE', #13038, #5739, #6849, .T. ) ;
#15010 = CARTESIAN_POINT ( 'NONE',  ( 8.552111707065320090, 3.043081950488160103, 5.304473962697122680 ) ) ;
#15011 = CARTESIAN_POINT ( 'NONE',  ( 51.19063959271458231, 0.000000000000000000, 70.12932606827693860 ) ) ;
#15012 = ADVANCED_FACE ( 'NONE', ( #7000 ), #9252, .F. ) ;
#15013 = CARTESIAN_POINT ( 'NONE',  ( -29.89610458603408105, 15.00000000000000000, -151.5049534636450801 ) ) ;
#15014 = ADVANCED_FACE ( 'NONE', ( #13976 ), #12135, .T. ) ;
#15015 = CARTESIAN_POINT ( 'NONE',  ( -2.298097038856278029, 4.625000000000000888, -1.201902961143720638 ) ) ;
#15016 = ORIENTED_EDGE ( 'NONE', *, *, #4424, .F. ) ;
#15017 = CARTESIAN_POINT ( 'NONE',  ( 1.052436484934202499, -2.075239479414269894, -1.000000000000000888 ) ) ;
#15018 = CARTESIAN_POINT ( 'NONE',  ( 10.63021595323582069, 2.452426006596266195, -106.2019669008089409 ) ) ;
#15019 = DIRECTION ( 'NONE',  ( -0.000000000000000000, -1.000000000000000000, -0.000000000000000000 ) ) ;
#15020 = CARTESIAN_POINT ( 'NONE',  ( 2.298097038856278473, 10.62500000000000000, -5.798097038856279362 ) ) ;
#15021 = CARTESIAN_POINT ( 'NONE',  ( 8.976503672017095425, 12.42208448007280275, 0.9787777583466945597 ) ) ;
#15022 = LINE ( 'NONE', #13930, #5691 ) ;
#15023 = CARTESIAN_POINT ( 'NONE',  ( 3.249999999999998224, 14.18750000000000178, -4.846194077712561388 ) ) ;
#15024 = APPROVAL ( #12326, 'UNSPECIFIED' ) ;
#15025 = CARTESIAN_POINT ( 'NONE',  ( 30.32986759126112730, 0.7500000000000000000, 46.54214087805580391 ) ) ;
#15026 = CARTESIAN_POINT ( 'NONE',  ( 2.651650429449553759, 14.87500000000000178, -0.8483495705504471296 ) ) ;
#15027 = CARTESIAN_POINT ( 'NONE',  ( -29.69515346086420138, 9.999999999999998224, -156.7390981038714983 ) ) ;
#15028 = CARTESIAN_POINT ( 'NONE',  ( -8.765409998386077817, 2.075239479414269450, -35.06535713112702979 ) ) ;
#15029 = DIRECTION ( 'NONE',  ( 0.000000000000000000, 0.000000000000000000, 1.000000000000000000 ) ) ;
#15030 = CARTESIAN_POINT ( 'NONE',  ( 30.32986759126112730, 1.750000000000000000, 43.04214087805580391 ) ) ;
#15031 = DIRECTION ( 'NONE',  ( 0.000000000000000000, 1.000000000000000000, 0.000000000000000000 ) ) ;
#15032 = CARTESIAN_POINT ( 'NONE',  ( 2.298097038856278473, 7.625000000000000000, -5.798097038856279362 ) ) ;
#15033 = CARTESIAN_POINT ( 'NONE',  ( 2.806001675047999022, 0.2533870648575867746, 1.824864976002073202 ) ) ;
#15034 = CARTESIAN_POINT ( 'NONE',  ( 8.602821479119551640, 5.000000000000001776, -113.5763767534210587 ) ) ;
#15035 = ORIENTED_EDGE ( 'NONE', *, *, #9785, .T. ) ;
#15036 = ORIENTED_EDGE ( 'NONE', *, *, #10815, .F. ) ;
#15037 = DIRECTION ( 'NONE',  ( -0.000000000000000000, 1.000000000000000000, -0.000000000000000000 ) ) ;
#15038 = CARTESIAN_POINT ( 'NONE',  ( -3.750000000000000000, 14.68750000000000178, -1.946699141100893149 ) ) ;
#15039 = CARTESIAN_POINT ( 'NONE',  ( -3.249999999999999112, 13.68750000000000178, -2.153805922287440833 ) ) ;
#15040 = CARTESIAN_POINT ( 'NONE',  ( 37.32986759126112730, 0.000000000000000000, 43.04214087805580391 ) ) ;
#15041 = ORIENTED_EDGE ( 'NONE', *, *, #6168, .T. ) ;
#15042 = CARTESIAN_POINT ( 'NONE',  ( -3.249999999999999556, 7.312500000000000888, -4.846194077712557835 ) ) ;
#15043 = CARTESIAN_POINT ( 'NONE',  ( -3.249999999999999556, 13.31250000000000000, -4.846194077712557835 ) ) ;
#15044 = CARTESIAN_POINT ( 'NONE',  ( -2.869987474717050624, 2.075239479414269894, -1.000000000000000888 ) ) ;
#15045 = CARTESIAN_POINT ( 'NONE',  ( -8.735813531966259760, 12.24413591761513054, -104.9486082961802680 ) ) ;
#15046 = CARTESIAN_POINT ( 'NONE',  ( -8.923457816049095825, 12.80882171512263312, -116.0747321664441074 ) ) ;
#15047 = SECURITY_CLASSIFICATION_LEVEL ( 'unclassified' ) ;
#15048 = CARTESIAN_POINT ( 'NONE',  ( 10.31224696326443535, 14.99999999999627320, -121.0233796642843913 ) ) ;
#15049 = CARTESIAN_POINT ( 'NONE',  ( -0.2500000000000000555, 4.500000000000000888, 1.500000000000000222 ) ) ;
#15050 = ORIENTED_EDGE ( 'NONE', *, *, #4694, .T. ) ;
#15051 = AXIS2_PLACEMENT_3D ( 'NONE', #5336, #9898, #2942 ) ;
#15052 = CARTESIAN_POINT ( 'NONE',  ( 26.60417991234133339, 3.130032034377395522, -138.2748749807007016 ) ) ;
#15053 = CARTESIAN_POINT ( 'NONE',  ( 3.249999999999999112, 9.812500000000000000, -2.153805922287439945 ) ) ;
#15054 = ORIENTED_EDGE ( 'NONE', *, *, #3564, .F. ) ;
#15055 = VERTEX_POINT ( 'NONE', #5837 ) ;
#15056 = CARTESIAN_POINT ( 'NONE',  ( 3.249999999999999112, 4.812500000000000888, -2.153805922287439945 ) ) ;
#15057 = CARTESIAN_POINT ( 'NONE',  ( 29.24464190187102375, 8.773889247172311556, -45.46299734238769474 ) ) ;
#15058 = CARTESIAN_POINT ( 'NONE',  ( -2.651650429449553314, 0.8750000000000000000, -6.151650429449552426 ) ) ;
#15059 = CARTESIAN_POINT ( 'NONE',  ( -3.249999999999999112, 5.812500000000000888, -4.846194077712558723 ) ) ;
#15060 = ORIENTED_EDGE ( 'NONE', *, *, #13276, .T. ) ;
#15061 = CARTESIAN_POINT ( 'NONE',  ( -0.1824722430594065969, 1.750000000000737410, 41.93241979182633372 ) ) ;
#15062 = DIRECTION ( 'NONE',  ( -0.000000000000000000, -1.000000000000000000, -0.000000000000000000 ) ) ;
#15063 = CARTESIAN_POINT ( 'NONE',  ( -3.749999999999999556, 5.187500000000001776, -1.946699141100892927 ) ) ;
#15064 = CARTESIAN_POINT ( 'NONE',  ( -25.70158769154330258, 0.8049789667686304551, -204.9870591480219844 ) ) ;
#15065 = CARTESIAN_POINT ( 'NONE',  ( -4.843886036682795826, 10.00000000000000178, -144.0640150611854438 ) ) ;
#15066 =( BOUNDED_SURFACE ( )  B_SPLINE_SURFACE ( 3, 2, ( 
 ( #14963, #8836, #8988 ),
 ( #13786, #5359, #12697 ),
 ( #11304, #6668, #3042 ),
 ( #6596, #10296, #6520 ),
 ( #2034, #4356, #11459 ),
 ( #5507, #10151, #947 ) ),
 .UNSPECIFIED., .F., .F., .T. ) 
 B_SPLINE_SURFACE_WITH_KNOTS ( ( 4, 2, 4 ),
 ( 3, 3 ),
 ( -2.081668171172168513E-17, 0.008318652500447831777, 0.01663730500089568437 ),
 ( 0.000000000000000000, 1.000000000000000000 ),
 .UNSPECIFIED. ) 
 GEOMETRIC_REPRESENTATION_ITEM ( )  RATIONAL_B_SPLINE_SURFACE ( (
 ( 1.000000000000000000, 0.7071067811865475727, 1.000000000000000000),
 ( 1.000000000000000000, 0.7071067811865475727, 1.000000000000000000),
 ( 1.000000000000000000, 0.7071067811865475727, 1.000000000000000000),
 ( 1.000000000000000000, 0.7071067811865475727, 1.000000000000000000),
 ( 1.000000000000000000, 0.7071067811865475727, 1.000000000000000000),
 ( 1.000000000000000000, 0.7071067811865475727, 1.000000000000000000) ) ) 
 REPRESENTATION_ITEM ( '' )  SURFACE ( )  );
#15067 = APPROVAL_ROLE ( '' ) ;
#15068 = CARTESIAN_POINT ( 'NONE',  ( -4.827512413385830037, 0.9636447990543512976, -1.000000000000001332 ) ) ;
#15069 = LOCAL_TIME ( 12, 28, 20.00000000000000000, #4762 ) ;
#15070 = EDGE_LOOP ( 'NONE', ( #8937, #13843, #3285, #8533 ) ) ;
#15071 = VECTOR ( 'NONE', #6143, 1000.000000000000000 ) ;
#15072 = CARTESIAN_POINT ( 'NONE',  ( 1.346194077712558279, 8.062500000000001776, -6.750000000000000888 ) ) ;
#15073 = CARTESIAN_POINT ( 'NONE',  ( -5.309262520577839872, 6.000000000000000000, -125.0911079416483176 ) ) ;
#15074 = CARTESIAN_POINT ( 'NONE',  ( 3.749999999999999556, 9.250000000000001776, -3.500000000000000444 ) ) ;
#15075 = CARTESIAN_POINT ( 'NONE',  ( 1.553300858899105963, 12.56250000000000000, -7.250000000000000000 ) ) ;
#15076 = LOCAL_TIME ( 12, 28, 20.00000000000000000, #32 ) ;
#15077 = ADVANCED_FACE ( 'NONE', ( #1201 ), #3501, .T. ) ;
#15078 = CARTESIAN_POINT ( 'NONE',  ( -66.14848843925153687, 14.98207687019956680, -197.4208877442913206 ) ) ;
#15079 = CARTESIAN_POINT ( 'NONE',  ( 1.320501113854931408, 5.000000000000000888, -137.8664870916819893 ) ) ;
#15080 = CARTESIAN_POINT ( 'NONE',  ( -3.749999999999999556, 12.74999999999999822, -3.499999999999999112 ) ) ;
#15081 = AXIS2_PLACEMENT_3D ( 'NONE', #1716, #14803, #13555 ) ;
#15082 = CARTESIAN_POINT ( 'NONE',  ( -2.739138985622725286, 4.336808689942017736E-16, -111.5297549026598176 ) ) ;
#15083 = VECTOR ( 'NONE', #5744, 1000.000000000000000 ) ;
#15084 = APPROVAL_STATUS ( 'not_yet_approved' ) ;
#15085 = DIRECTION ( 'NONE',  ( 0.000000000000000000, 1.000000000000000000, 0.000000000000000000 ) ) ;
#15086 = ORIENTED_EDGE ( 'NONE', *, *, #9004, .F. ) ;
#15087 = DIRECTION ( 'NONE',  ( 0.000000000000000000, 1.000000000000000000, 0.000000000000000000 ) ) ;
#15088 = CARTESIAN_POINT ( 'NONE',  ( 1.831246893856136593, -2.490287375297125294, -1.000000000000021760 ) ) ;
#15089 = CARTESIAN_POINT ( 'NONE',  ( -52.20743557211550723, 15.00000000000133049, -168.0633964594969143 ) ) ;
#15090 = APPROVAL ( #2923, 'UNSPECIFIED' ) ;
#15091 = AXIS2_PLACEMENT_3D ( 'NONE', #8601, #5290, #1426 ) ;
#15092 = CARTESIAN_POINT ( 'NONE',  ( 2.298097038856279362, 3.375000000000000444, -1.201902961143720860 ) ) ;
#15093 = ORIENTED_EDGE ( 'NONE', *, *, #15271, .T. ) ;
#15094 = CARTESIAN_POINT ( 'NONE',  ( -8.431010172942514203, 9.999999999999998224, -122.5582262043254076 ) ) ;
#15095 = CARTESIAN_POINT ( 'NONE',  ( -17.48539614069081694, 15.00000000000000178, -148.4416824785454878 ) ) ;
#15096 = VECTOR ( 'NONE', #10190, 1000.000000000000000 ) ;
#15097 = CARTESIAN_POINT ( 'NONE',  ( 8.881162068611669014, 11.71160396371214496, 5.347396915146337193 ) ) ;
#15098 = CARTESIAN_POINT ( 'NONE',  ( -2.424117392950516869, 5.000000000000000888, -107.6599666633565988 ) ) ;
#15099 = CARTESIAN_POINT ( 'NONE',  ( 1.346194077712558279, 13.06250000000000178, -6.750000000000000888 ) ) ;
#15100 = ADVANCED_FACE ( 'NONE', ( #10557 ), #3252, .T. ) ;
#15101 = CARTESIAN_POINT ( 'NONE',  ( 27.13166404935670073, 8.673617379884035472E-16, -138.0564292571840213 ) ) ;
#15102 = CARTESIAN_POINT ( 'NONE',  ( -2.651650429449553314, 1.874999999999999778, -6.151650429449552426 ) ) ;
#15103 = DIRECTION ( 'NONE',  ( 0.08794243244723007336, 0.000000000000000000, 0.9961255586397049777 ) ) ;
#15104 = EDGE_CURVE ( 'NONE', #2695, #6374, #5398, .T. ) ;
#15105 = AXIS2_PLACEMENT_3D ( 'NONE', #14935, #11508, #11349 ) ;
#15106 = DIRECTION ( 'NONE',  ( 0.08794243244722425856, 0.000000000000000000, 0.9961255586397054218 ) ) ;
#15107 = CARTESIAN_POINT ( 'NONE',  ( 1.004809442601927394, 5.000000000000000888, -139.4752805618705622 ) ) ;
#15108 = CARTESIAN_POINT ( 'NONE',  ( -5.836568743579779728, 0.000000000000000000, 17.25548782215969368 ) ) ;
#15109 = CARTESIAN_POINT ( 'NONE',  ( -3.980102097228897245E-16, 9.500000000000000000, -6.749999999999999112 ) ) ;
#15110 = CARTESIAN_POINT ( 'NONE',  ( 43.24549764042590994, 1.750000000004062306, 51.33556869416222668 ) ) ;
#15111 = APPLICATION_CONTEXT ( 'configuration controlled 3d designs of mechanical parts and assemblies' ) ;
#15112 = CARTESIAN_POINT ( 'NONE',  ( -8.886921396801799489, 9.999999999999998224, -105.5168766094550250 ) ) ;
#15113 = VERTEX_POINT ( 'NONE', #8306 ) ;
#15114 = PRODUCT_DEFINITION_SHAPE ( 'NONE', 'NONE',  #8846 ) ;
#15115 = EDGE_LOOP ( 'NONE', ( #3858, #3666 ) ) ;
#15116 = PLANE ( 'NONE',  #2575 ) ;
#15117 = CARTESIAN_POINT ( 'NONE',  ( -4.592425496802573972E-16, 15.00000000000000178, -7.250000000000000000 ) ) ;
#15118 = CARTESIAN_POINT ( 'NONE',  ( 3.749999999999998668, 1.187499999999999778, -5.053300858899108405 ) ) ;
#15119 = CARTESIAN_POINT ( 'NONE',  ( 7.353370788917347411, 14.99999999999197264, -111.8370434415751475 ) ) ;
#15120 = EDGE_LOOP ( 'NONE', ( #13788, #10212, #7456, #12953 ) ) ;
#15121 = CARTESIAN_POINT ( 'NONE',  ( -2.298097038856278473, 14.12500000000000000, -1.201902961143720416 ) ) ;
#15122 = CARTESIAN_POINT ( 'NONE',  ( -0.8684534520279959535, 5.000000000000001776, -104.6281219612548341 ) ) ;
#15123 = EDGE_CURVE ( 'NONE', #7276, #13215, #964, .T. ) ;
#15124 = CARTESIAN_POINT ( 'NONE',  ( -9.285933603414303406, 9.999999999999996447, -105.1819416496436475 ) ) ;
#15125 = CARTESIAN_POINT ( 'NONE',  ( 1.346194077712558057, 5.562500000000000000, -6.750000000000000000 ) ) ;
#15126 = APPROVAL_DATE_TIME ( #9375, #12916 ) ;
#15127 = AXIS2_PLACEMENT_3D ( 'NONE', #11511, #5207, #4056 ) ;
#15128 = CARTESIAN_POINT ( 'NONE',  ( 10.88443679120024399, 8.773889247172311556, -40.61244394157877480 ) ) ;
#15129 = DIRECTION ( 'NONE',  ( 0.000000000000000000, 0.000000000000000000, 1.000000000000000000 ) ) ;
#15130 = VERTEX_POINT ( 'NONE', #3675 ) ;
#15131 = CARTESIAN_POINT ( 'NONE',  ( 1.260825460258694797, 4.119514498333133545, -139.4012524756404332 ) ) ;
#15132 = CARTESIAN_POINT ( 'NONE',  ( 2.298097038856278473, 12.62500000000000000, -5.798097038856279362 ) ) ;
#15133 = EDGE_LOOP ( 'NONE', ( #5367, #9596, #11326, #8301 ) ) ;
#15134 = ORIENTED_EDGE ( 'NONE', *, *, #6925, .T. ) ;
#15135 = CARTESIAN_POINT ( 'NONE',  ( -2.651650429449552870, 11.62500000000000000, -0.8483495705504463524 ) ) ;
#15136 = CARTESIAN_POINT ( 'NONE',  ( -26.52470037256358992, 4.000000000000000000, -207.7145413388536781 ) ) ;
#15137 = CARTESIAN_POINT ( 'NONE',  ( -1.553300858899107073, 1.937500000000000222, -7.249999999999999112 ) ) ;
#15138 = CARTESIAN_POINT ( 'NONE',  ( -3.980102097228897738E-16, 6.000000000000000888, -6.749999999999999112 ) ) ;
#15139 = ORIENTED_EDGE ( 'NONE', *, *, #9714, .F. ) ;
#15140 = CARTESIAN_POINT ( 'NONE',  ( 19.43417530611593591, 1.750000000000704325, 66.43326964946760427 ) ) ;
#15141 = CARTESIAN_POINT ( 'NONE',  ( 3.249999999999999556, 4.750000000000000000, -3.500000000000000000 ) ) ;
#15142 = CC_DESIGN_APPROVAL ( #1853, ( #9187 ) ) ;
#15143 = B_SPLINE_CURVE_WITH_KNOTS ( 'NONE', 3,
 ( #5722, #9508, #4721, #10667, #14159, #4571 ),
 .UNSPECIFIED., .F., .F.,
 ( 4, 2, 4 ),
 ( 0.000000000000000000, 0.0003771714294063781151, 0.0007543428588127562302 ),
 .UNSPECIFIED. ) ;
#15144 = CARTESIAN_POINT ( 'NONE',  ( 2.651650429449552870, 5.625000000000000000, -6.151650429449554203 ) ) ;
#15145 = CARTESIAN_POINT ( 'NONE',  ( -25.55455346258773375, 2.452721150094688607, -207.9965800587423814 ) ) ;
#15146 = CARTESIAN_POINT ( 'NONE',  ( 8.058837131447921465, 10.00000000000000000, -130.1898991670217640 ) ) ;
#15147 = AXIS2_PLACEMENT_3D ( 'NONE', #12524, #6950, #12832 ) ;
#15148 = COORDINATED_UNIVERSAL_TIME_OFFSET ( 0, 0, .AHEAD. ) ;
#15149 = CARTESIAN_POINT ( 'NONE',  ( 25.37775455676784730, 5.000000000000000888, -136.0262733555301224 ) ) ;
#15150 = EDGE_LOOP ( 'NONE', ( #9367, #1330, #9163, #7123 ) ) ;
#15151 = CARTESIAN_POINT ( 'NONE',  ( 0.000000000000000000, 6.500000000000000000, -0.2500000000000002220 ) ) ;
#15152 = CARTESIAN_POINT ( 'NONE',  ( -4.122964195042671420, 10.00000000000000355, -110.0534507760547314 ) ) ;
#15153 = AXIS2_PLACEMENT_3D ( 'NONE', #14912, #14835, #5682 ) ;
#15155 =( BOUNDED_SURFACE ( )  B_SPLINE_SURFACE ( 3, 2, ( 
 ( #3246, #6729, #864 ),
 ( #3100, #7958, #13844 ),
 ( #6653, #6803, #11519 ),
 ( #5494, #10213, #10352 ),
 ( #15094, #10806, #11737 ),
 ( #13140, #5021, #9502 ),
 ( #7023, #10736, #12910 ),
 ( #14071, #7327, #10579 ),
 ( #9571, #9653, #2324 ),
 ( #150, #2550, #8408 ),
 ( #3474, #12845, #6089 ),
 ( #11809, #14384, #10890 ),
 ( #1225, #8329, #221 ),
 ( #5936, #14299, #10660 ),
 ( #307, #4714, #13221 ),
 ( #75, #8186, #11965 ),
 ( #4860, #4787, #14225 ),
 ( #3784, #8490, #3698 ),
 ( #3626, #1157, #13055 ),
 ( #2624, #2468, #7165 ),
 ( #11886, #12039, #6012 ),
 ( #5860, #7250, #1388 ),
 ( #1460, #4936, #6169 ),
 ( #9426, #14152, #3552 ),
 ( #1309, #8259, #12986 ),
 ( #2391, #7088, #5325 ),
 ( #14468, #10038, #13298 ),
 ( #7715, #8803, #2932 ),
 ( #6332, #1852, #12431 ),
 ( #6557, #9885, #2701 ),
 ( #539, #463, #7635 ),
 ( #11047, #11270, #5174 ) ),
 .UNSPECIFIED., .F., .F., .F. ) 
 B_SPLINE_SURFACE_WITH_KNOTS ( ( 4, 2, 2, 2, 2, 2, 2, 2, 2, 2, 2, 2, 2, 2, 2, 4 ),
 ( 3, 3 ),
 ( -6.938893903907228378E-18, 0.004113674805128861474, 0.008227349610257729887, 0.01234102441538659917, 0.01336944311666881519, 0.01439786181795103294, 0.01645469922051546671, 0.01851153662307990222, 0.02056837402564433426, 0.02262521142820876976, 0.02365363012949098925, 0.02468204883077320527, 0.02879572363590207282, 0.02982414233718429231, 0.03085256103846650833, 0.03290939844103094036 ),
 ( 0.000000000000000000, 1.000000000000000000 ),
 .UNSPECIFIED. ) 
 GEOMETRIC_REPRESENTATION_ITEM ( )  RATIONAL_B_SPLINE_SURFACE ( (
 ( 1.000000000000000000, 0.7071067811865475727, 1.000000000000000000),
 ( 1.000000000000000000, 0.7071067811865475727, 1.000000000000000000),
 ( 1.000000000000000000, 0.7071067811865475727, 1.000000000000000000),
 ( 1.000000000000000000, 0.7071067811865475727, 1.000000000000000000),
 ( 1.000000000000000000, 0.7071067811865475727, 1.000000000000000000),
 ( 1.000000000000000000, 0.7071067811865475727, 1.000000000000000000),
 ( 1.000000000000000000, 0.7071067811865475727, 1.000000000000000000),
 ( 1.000000000000000000, 0.7071067811865475727, 1.000000000000000000),
 ( 1.000000000000000000, 0.7071067811865475727, 1.000000000000000000),
 ( 1.000000000000000000, 0.7071067811865475727, 1.000000000000000000),
 ( 1.000000000000000000, 0.7071067811865475727, 1.000000000000000000),
 ( 1.000000000000000000, 0.7071067811865475727, 1.000000000000000000),
 ( 1.000000000000000000, 0.7071067811865473507, 1.000000000000000000),
 ( 1.000000000000000000, 0.7071067811865473507, 1.000000000000000000),
 ( 1.000000000000000000, 0.7071067811865475727, 1.000000000000000000),
 ( 1.000000000000000000, 0.7071067811865475727, 1.000000000000000000),
 ( 1.000000000000000000, 0.7071067811865474617, 1.000000000000000000),
 ( 1.000000000000000000, 0.7071067811865474617, 1.000000000000000000),
 ( 1.000000000000000000, 0.7071067811865475727, 1.000000000000000000),
 ( 1.000000000000000000, 0.7071067811865475727, 1.000000000000000000),
 ( 1.000000000000000000, 0.7071067811865472397, 1.000000000000000000),
 ( 1.000000000000000000, 0.7071067811865472397, 1.000000000000000000),
 ( 1.000000000000000000, 0.7071067811865475727, 1.000000000000000000),
 ( 1.000000000000000000, 0.7071067811865475727, 1.000000000000000000),
 ( 1.000000000000000000, 0.7071067811865481278, 1.000000000000000000),
 ( 1.000000000000000000, 0.7071067811865481278, 1.000000000000000000),
 ( 1.000000000000000000, 0.7071067811865467956, 1.000000000000000000),
 ( 1.000000000000000000, 0.7071067811865467956, 1.000000000000000000),
 ( 1.000000000000000000, 0.7071067811865467956, 1.000000000000000000),
 ( 1.000000000000000000, 0.7071067811865467956, 1.000000000000000000),
 ( 1.000000000000000000, 0.7071067811865475727, 1.000000000000000000),
 ( 1.000000000000000000, 0.7071067811865475727, 1.000000000000000000) ) ) 
 REPRESENTATION_ITEM ( '' )  SURFACE ( )  );
#15154 = CARTESIAN_POINT ( 'NONE',  ( -3.750000000000000000, 8.812500000000001776, -5.053300858899105741 ) ) ;
#15156 = CARTESIAN_POINT ( 'NONE',  ( -31.09209721305616370, 5.000000000000000000, -156.3611406121567597 ) ) ;
#15157 = CARTESIAN_POINT ( 'NONE',  ( -67.57161933043941815, 13.62327337447829656, -200.3246758838251083 ) ) ;
#15158 = CARTESIAN_POINT ( 'NONE',  ( 0.1694250374747845456, 2.802173579811035431, -138.2948546871898259 ) ) ;
#15159 = CARTESIAN_POINT ( 'NONE',  ( 1.553300858899109516, 14.43750000000000178, 0.2499999999999993616 ) ) ;
#15160 = CARTESIAN_POINT ( 'NONE',  ( 0.000000000000000000, 5.000000000000000000, -3.500000000000000000 ) ) ;
#15161 = PERSON_AND_ORGANIZATION ( #3176, #3020 ) ;
#15162 =( BOUNDED_SURFACE ( )  B_SPLINE_SURFACE ( 3, 1, ( 
 ( #3932, #2856 ),
 ( #530, #6471 ),
 ( #1613, #6396 ),
 ( #2925, #5319 ) ),
 .UNSPECIFIED., .F., .F., .F. ) 
 B_SPLINE_SURFACE_WITH_KNOTS ( ( 4, 4 ),
 ( 2, 2 ),
 ( 0.000000000000000000, 1.000000000000000000 ),
 ( 0.000000000000000000, 1.000000000000000000 ),
 .UNSPECIFIED. ) 
 GEOMETRIC_REPRESENTATION_ITEM ( )  RATIONAL_B_SPLINE_SURFACE ( (
 ( 1.000000000000000000, 1.000000000000000000),
 ( 0.8656789684289789566, 0.8656789684289789566),
 ( 0.8656789684289789566, 0.8656789684289789566),
 ( 1.000000000000000000, 1.000000000000000000) ) ) 
 REPRESENTATION_ITEM ( '' )  SURFACE ( )  );
#15163 = CIRCLE ( 'NONE', #2065, 1.000000000000000888 ) ;
#15164 = DIRECTION ( 'NONE',  ( 0.000000000000000000, 1.000000000000000000, 0.000000000000000000 ) ) ;
#15165 = ORIENTED_EDGE ( 'NONE', *, *, #56, .F. ) ;
#15166 = CARTESIAN_POINT ( 'NONE',  ( 8.669753383557360138, 3.405435594033015878, 5.423001458801155472 ) ) ;
#15167 = CARTESIAN_POINT ( 'NONE',  ( -1.346194077712559167, 2.437500000000000444, -6.749999999999999112 ) ) ;
#15168 = ADVANCED_FACE ( 'NONE', ( #281 ), #8381, .F. ) ;
#15169 = CARTESIAN_POINT ( 'NONE',  ( -55.44729830701660944, 15.00000000001072920, -173.4678552871688453 ) ) ;
#15170 = EDGE_CURVE ( 'NONE', #14016, #13160, #6216, .T. ) ;
#15171 = CARTESIAN_POINT ( 'NONE',  ( -1.346194077712559167, 2.937500000000000444, -6.749999999999999112 ) ) ;
#15172 = ORIENTED_EDGE ( 'NONE', *, *, #9715, .T. ) ;
#15173 = CARTESIAN_POINT ( 'NONE',  ( 1.487533013587992059, -2.579141538380385956, -1.000000000000001110 ) ) ;
#15174 = CARTESIAN_POINT ( 'NONE',  ( -15.11050069331331613, 15.00000000000000000, -146.5097068764998198 ) ) ;
#15175 = CARTESIAN_POINT ( 'NONE',  ( 8.875022499991096936, 9.999999999999747757, 5.628716256677545715 ) ) ;
#15176 = AXIS2_PLACEMENT_3D ( 'NONE', #14566, #6507, #12458 ) ;
#15177 = CARTESIAN_POINT ( 'NONE',  ( -3.249999999999999556, 13.75000000000000000, -3.500000000000000000 ) ) ;
#15178 = VECTOR ( 'NONE', #14017, 1000.000000000000000 ) ;
#15179 = DIRECTION ( 'NONE',  ( -0.9997619372588931741, 0.000000000000000000, -0.02181900108494707127 ) ) ;
#15180 = CARTESIAN_POINT ( 'NONE',  ( 3.749999999999999112, 1.187500000000000222, -5.053300858899108405 ) ) ;
#15181 = DIRECTION ( 'NONE',  ( 0.000000000000000000, 1.000000000000000000, 0.000000000000000000 ) ) ;
#15182 = DIRECTION ( 'NONE',  ( -0.3090169943749621062, 0.000000000000000000, -0.9510565162951489793 ) ) ;
#15183 = B_SPLINE_CURVE_WITH_KNOTS ( 'NONE', 3,
 ( #15107, #7032, #10588, #5727 ),
 .UNSPECIFIED., .F., .F.,
 ( 4, 4 ),
 ( 0.000000000000000000, 1.000000000000000000 ),
 .UNSPECIFIED. ) ;
#15184 = DIRECTION ( 'NONE',  ( -1.225982338248072509E-13, 0.000000000000000000, -1.000000000000000000 ) ) ;
#15185 = FACE_OUTER_BOUND ( 'NONE', #10849, .T. ) ;
#15186 = CARTESIAN_POINT ( 'NONE',  ( 2.298097038856279362, 11.87500000000000000, -1.201902961143720860 ) ) ;
#15187 = CARTESIAN_POINT ( 'NONE',  ( 4.374104445798832508, 15.00089282178849182, -1.804052482945245783 ) ) ;
#15188 = CARTESIAN_POINT ( 'NONE',  ( -17.32624372124044854, 0.6199615622964459449, -130.2318118670719116 ) ) ;
#15189 = ORIENTED_EDGE ( 'NONE', *, *, #6455, .F. ) ;
#15190 = EDGE_CURVE ( 'NONE', #7952, #5770, #13520, .T. ) ;
#15191 = VERTEX_POINT ( 'NONE', #511 ) ;
#15192 = LINE ( 'NONE', #4585, #4513 ) ;
#15193 = CARTESIAN_POINT ( 'NONE',  ( -3.749999999999999556, 3.187500000000000000, -1.946699141100892927 ) ) ;
#15194 = CARTESIAN_POINT ( 'NONE',  ( -2.298097038856278029, 14.62500000000000178, -1.201902961143720638 ) ) ;
#15195 = VECTOR ( 'NONE', #10206, 1000.000000000000000 ) ;
#15196 = EDGE_CURVE ( 'NONE', #14503, #12741, #3744, .T. ) ;
#15197 = EDGE_LOOP ( 'NONE', ( #8029, #267, #7424, #10093 ) ) ;
#15198 = CARTESIAN_POINT ( 'NONE',  ( -2.298097038856278029, 1.625000000000000000, -1.201902961143720638 ) ) ;
#15199 = CARTESIAN_POINT ( 'NONE',  ( -51.71514206936258518, 9.999999999999998224, -145.7302012135338884 ) ) ;
#15200 = CARTESIAN_POINT ( 'NONE',  ( -9.243017000006215511, 10.73487358288918436, -105.1634759883721273 ) ) ;
#15201 = CARTESIAN_POINT ( 'NONE',  ( -1.346194077712559389, 4.437500000000000888, -6.749999999999999112 ) ) ;
#15202 = COORDINATED_UNIVERSAL_TIME_OFFSET ( 0, 0, .AHEAD. ) ;
#15203 = CC_DESIGN_PERSON_AND_ORGANIZATION_ASSIGNMENT ( #6902, #3506, ( #4938 ) ) ;
#15204 = CARTESIAN_POINT ( 'NONE',  ( 10.82638304870340029, 12.49999999999999822, -107.3456397791438235 ) ) ;
#15205 = CARTESIAN_POINT ( 'NONE',  ( 5.228075279701640099, 1.000000000000000000, -165.7939279834373849 ) ) ;
#15206 = EDGE_LOOP ( 'NONE', ( #12329, #11098, #3827 ) ) ;
#15207 = DIRECTION ( 'NONE',  ( 1.000000000000000000, -0.000000000000000000, 0.000000000000000000 ) ) ;
#15208 = CARTESIAN_POINT ( 'NONE',  ( -3.249999999999999556, 10.31250000000000000, -4.846194077712557835 ) ) ;
#15209 = VERTEX_POINT ( 'NONE', #12324 ) ;
#15210 = ADVANCED_FACE ( 'NONE', ( #8849 ), #7841, .F. ) ;
#15211 = ORIENTED_EDGE ( 'NONE', *, *, #14349, .T. ) ;
#15212 = CARTESIAN_POINT ( 'NONE',  ( 2.651650429449554203, 9.374999999999998224, -0.8483495705504471296 ) ) ;
#15213 = CARTESIAN_POINT ( 'NONE',  ( 9.044950117654433797, -4.000000000000000000, -137.9826476090360643 ) ) ;
#15214 = CARTESIAN_POINT ( 'NONE',  ( 3.749999999999999112, 4.187500000000000888, -5.053300858899108405 ) ) ;
#15215 = ADVANCED_FACE ( 'NONE', ( #7689 ), #1970, .T. ) ;
#15216 = CARTESIAN_POINT ( 'NONE',  ( 2.298097038856278029, 8.125000000000000000, -5.798097038856279362 ) ) ;
#15218 = EDGE_CURVE ( 'NONE', #10617, #1079, #10088, .T. ) ;
#15217 = ORIENTED_EDGE ( 'NONE', *, *, #8627, .T. ) ;
#15219 = CARTESIAN_POINT ( 'NONE',  ( 1.814459646441706209, 14.99999999999999822, -110.3167319592368329 ) ) ;
#15220 = CARTESIAN_POINT ( 'NONE',  ( -1.346194077712559389, 2.062500000000000000, -0.2500000000000002220 ) ) ;
#15221 = CARTESIAN_POINT ( 'NONE',  ( -1.553300858899107295, 5.437500000000002665, -7.250000000000000000 ) ) ;
#15222 = CARTESIAN_POINT ( 'NONE',  ( -25.17932510765911047, 0.9650723256931513783, -205.4209994318837857 ) ) ;
#15223 = DIRECTION ( 'NONE',  ( 0.9997619372588932851, 0.000000000000000000, 0.02181900108494707821 ) ) ;
#15224 = SECURITY_CLASSIFICATION_LEVEL ( 'unclassified' ) ;
#15225 = DIRECTION ( 'NONE',  ( -0.000000000000000000, 1.000000000000000000, -0.000000000000000000 ) ) ;
#15226 = DIRECTION ( 'NONE',  ( -1.000000000000000000, 0.000000000000000000, 0.000000000000000000 ) ) ;
#15227 = ORIENTED_EDGE ( 'NONE', *, *, #7627, .T. ) ;
#15228 = CARTESIAN_POINT ( 'NONE',  ( -1.346194077712559167, 6.937500000000001776, -6.749999999999999112 ) ) ;
#15229 = CARTESIAN_POINT ( 'NONE',  ( 4.248871783098665311, 6.000000000000000000, -126.1456066832003842 ) ) ;
#15230 = CC_DESIGN_PERSON_AND_ORGANIZATION_ASSIGNMENT ( #10961, #6394, ( #10666 ) ) ;
#15231 = CARTESIAN_POINT ( 'NONE',  ( -3.749999999999999556, 7.750000000000000888, -3.499999999999999112 ) ) ;
#15232 = CARTESIAN_POINT ( 'NONE',  ( -4.592425496802573972E-16, 11.50000000000000000, -7.249999999999999112 ) ) ;
#15233 = CARTESIAN_POINT ( 'NONE',  ( -64.24125335076371357, 14.99999999999999645, -182.1877858736318103 ) ) ;
#15234 = CARTESIAN_POINT ( 'NONE',  ( -4.853391382351440519, -0.9800309627322401074, -1.000000000000001110 ) ) ;
#15235 = CARTESIAN_POINT ( 'NONE',  ( -3.249999999999999556, 8.312500000000000000, -4.846194077712557835 ) ) ;
#15236 = CARTESIAN_POINT ( 'NONE',  ( 3.249999999999998224, 0.1875000000000000833, -4.846194077712561388 ) ) ;
#15237 = LINE ( 'NONE', #15160, #6763 ) ;
#15238 = APPROVAL_DATE_TIME ( #1299, #8378 ) ;
#15239 = CARTESIAN_POINT ( 'NONE',  ( 9.991434137473303778, 4.873277969712327184, -45.52604821315951966 ) ) ;
#15240 = ORIENTED_EDGE ( 'NONE', *, *, #7718, .F. ) ;
#15241 = CARTESIAN_POINT ( 'NONE',  ( -27.33151177440234392, 4.000000000000656364, -206.5142783688401948 ) ) ;
#15242 = CARTESIAN_POINT ( 'NONE',  ( 2.298097038856279362, 4.875000000000000000, -1.201902961143720860 ) ) ;
#15243 = CARTESIAN_POINT ( 'NONE',  ( -68.23215113762095996, 15.00000000000000000, -203.6364912936910798 ) ) ;
#15244 = CARTESIAN_POINT ( 'NONE',  ( 2.298097038856279362, 7.375000000000000000, -1.201902961143720860 ) ) ;
#15245 = EDGE_LOOP ( 'NONE', ( #14971, #2300, #2883, #4764 ) ) ;
#15246 = DIRECTION ( 'NONE',  ( 1.000000000000000000, 0.000000000000000000, 0.000000000000000000 ) ) ;
#15247 =( BOUNDED_SURFACE ( )  B_SPLINE_SURFACE ( 3, 2, ( 
 ( #8262, #12991, #11740, #8492, #1160, #3702, #154, #14302, #1312, #6094, #9575, #13143, #12914, #11889, #14156, #8188, #2327, #4791, #7027, #2472, #2395, #5940, #9656, #1230, #10809, #5863, #225, #10582, #2226, #9430, #79, #4940, #4719, #9505, #13224, #14229, #3631, #13058, #7169, #6017, #10739, #2553, #7253, #11971, #14387, #9742, #8878, #1623, #1693, #12354, #9964, #1774, #3943, #14627, #6174, #14471, #13381, #7638, #11050, #12283, #6483, #7404, #6336, #2934, #13461, #310, #14548, #5254, #4024, #2787, #10974, #3867, #8569, #12042, #11200, #5024, #541, #13610, #3012, #622, #5328, #13301, #4104, #10040, #5101, #7489, #466, #14777, #1463, #2704, #12129, #8805, #1545, #6258, #4174, #9815, #392, #5179, #13535, #12207, #8645, #10894, #6404, #8729, #9889, #2865, #7564, #14703, #11122, #694, #1855, #6560, #11273, #12433, #7719, #2119, #888, #15042, #10382, #11472, #5592, #12513, #6794, #851, #924, #1072, #12821, #5483, #9035, #8958, #8024, #9263, #2229, #15235, #777, #3155, #12589, #2006, #6717, #11429, #6242, #2979, #10822, #239, #6384, #12099, #13118, #129, #370, #7306, #5080, #5153, #13355, #1367, #6070, #4916, #10950, #9793, #14363, #3763, #14523, #3103, #13774, #1875, #6580, #11368, #12681, #10216, #5569, #10354, #15020, #4410, #7099, #13235, #11899, #7339, #3876, #652, #7789, #11338, #11188, #12553, #12785, #10463, #14296, #9499, #13900, #11639, #2225, #5778, #2699, #10969, #6087, #4019, #4857, #14540, #14295, #7484, #14382, #6253, #2780, #7248, #8488, #461, #3938, #7325, #5171, #9568, #13296, #2621, #387, #9737, #12202, #1689, #3781, #6330, #9883, #11045, #13219, #7398, #14621, #8639, #9650, #8722, #12121, #12279, #12037, #9809, #8560, #7560, #13456, #6400, #1539, #1618, #218, #14466, #147, #5096, #13375, #2860, #3695 ),
 ( #11962, #8404, #1458, #13136, #1386, #3862, #2547, #10804, #6165, #5019, #4934, #10887, #305, #536, #4098, #14927, #7940, #12659, #11422, #845, #4249, #14773, #2076, #14849, #1850, #8950, #9099, #11114, #12349, #2930, #3147, #6478, #5323, #14994, #4170, #8874, #5395, #7861, #6555, #13605, #5250, #11341, #13680, #3079, #4392, #1767, #4323, #14697, #13821, #7793, #11267, #12503, #3007, #7712, #690, #6709, #5547, #767, #9960, #12429, #8801, #10110, #1921, #6633, #3225, #10262, #7633, #11195, #13531, #5474, #10193, #9027, #618, #10036, #13752, #12581, #1995, #15298, #5843, #3307, #2301, #4549, #11500, #13909, #10496, #9178, #8164, #9256, #11647, #271, #12813, #7293, #915, #12006, #10332, #986, #15151, #13982, #10852, #12742, #3378, #14433, #9701, #15228, #5618, #13265, #7006, #8088, #11720, #9406, #4689, #1432, #4468, #3830, #1064, #1140, #6138, #14131, #4985, #2221, #9332, #15072, #8016, #6930, #2592, #5773, #10563, #8531, #2151, #4620, #12968, #12892, #6855, #14052, #3530, #3451, #8240, #5696, #11569, #10416, #6788, #8842, #13569, #11016, #503, #2970, #11163, #12171, #1816, #5221, #14816, #1588, #12316, #11084, #10081, #6527, #8918, #4070, #4142, #2750, #1659, #2670, #9931, #2900, #584, #8771, #3911, #6372, #6446, #14511, #1509, #8607, #5297, #6221, #14666, #4213, #13503, #14585, #10009, #431, #11241, #7370, #7601, #9852, #6299, #3987, #7454, #1734, #14743, #7682, #12395, #354, #5141, #660, #12085, #5365, #12249, #10936, #8692, #13427, #13342, #5067, #2831, #9779, #7531, #953, #9071, #2041, #5658, #11390, #7760, #15039, #6753, #4587, #5587, #6822, #9218, #12703, #10301, #4433, #10236, #7982, #14969, #4290, #11465, #8994, #15194, #9144, #13647, #3049, #11538, #13869, #4509, #6892, #3269, #12474, #885, #1892, #2116, #11311, #7835 ),
 ( #11612, #6602, #14892, #5437, #10379, #13722, #12549, #2188, #6675, #1960, #7902, #15118, #4362, #812, #732, #13948, #3345, #8053, #1031, #3121, #12781, #10157, #5514, #5737, #13792, #10456, #3190, #12627, #7187, #9525, #9594, #2493, #8351, #5812, #4811, #7041, #14019, #1107, #13008, #11689, #10681, #11758, #14176, #2574, #20, #14322, #3416, #3726, #12855, #3498, #2345, #1178, #13164, #15265, #5879, #1411, #11988, #2413, #8126, #247, #14246, #10599, #3648, #11910, #1335, #8431, #6973, #6116, #3578, #13077, #7274, #6038, #10829, #4736, #11829, #2268, #10532, #9447, #4882, #8280, #10758, #9294, #4656, #7109, #175, #99, #9365, #1253, #14095, #5959, #8204, #12935, #2649, #1482, #4962, #11144, #13246, #8749, #1792, #6506, #5274, #9985, #13401, #8587, #11221, #8670, #10993, #2805, #2951, #9677, #6197, #12064, #12299, #331, #14490, #8824, #13320, #2725, #14565, #1711, #409, #7428, #14408, #5198, #7510, #12228, #13551, #10913, #13481, #8511, #7659, #1639, #5118, #6354, #12147, #1564, #9833, #563, #14723, #9912, #3807, #6279, #7351, #3964, #11067, #484, #12375, #4123, #5045, #9761, #3888, #14646, #4043, #2881, #7582, #6425, #640, #10061, #5344, #14797, #4192, #8898, #502, #270, #12315, #12005, #3829, #6371, #1431, #430, #10008, #8691, #9778, #1658, #6220, #1733, #14742, #1587, #5066, #7369, #14510, #13264, #12248, #11083, #11015, #13425, #10851, #10935, #12169, #4141, #5220, #7453, #9930, #3910, #353, #8530, #5296, #2669, #14664, #4069, #8770, #8606, #6298, #13502, #13341, #7292, #14584, #5140, #13185, #9851, #2899, #7600, #6445, #3986, #2830, #2749, #7530, #11162, #12084, #582, #1508, #2591, #6137, #4984, #9699, #14432, #10235, #15038, #2115, #5512, #7681, #1959, #15117, #811, #6526, #3047, #952, #13721, #11389, #4361, #14815 ),
 ( #4212, #7759, #12702, #1891, #12473, #3120, #5586, #14891, #6601, #8841, #9070, #14968, #6674, #6821, #8917, #2040, #12394, #11537, #12548, #4288, #13791, #11310, #731, #8993, #4432, #3268, #3189, #13568, #5436, #10156, #11240, #5364, #2969, #9143, #1814, #12626, #5657, #10378, #13868, #7980, #7901, #7834, #659, #6751, #11464, #884, #10080, #13646, #10300, #11611, #11828, #15193, #14018, #8350, #12854, #8125, #14094, #1252, #10531, #2267, #4508, #4735, #7040, #12933, #13076, #10454, #13007, #8052, #7186, #8203, #15264, #1177, #6972, #11687, #4655, #97, #14245, #9446, #10757, #1106, #13947, #5811, #9364, #3497, #11909, #9524, #1030, #4586, #9216, #14174, #2344, #2412, #6037, #3577, #8279, #9293, #4810, #7108, #5958, #5736, #19, #11757, #3344, #3415, #5878, #6891, #10598, #10680, #3647, #2492, #1334, #12780, #2187, #483, #3725, #9676, #8510, #2648, #4042, #6115, #12063, #7581, #2880, #3887, #4881, #6424, #408, #7350, #5117, #2804, #8669, #5197, #13163, #12298, #5043, #9832, #9911, #13400, #14645, #1481, #2724, #9593, #2572, #6196, #11066, #14489, #14564, #8747, #10828, #9760, #6353, #1563, #8430, #10912, #7508, #7427, #330, #11987, #246, #174, #3963, #8586, #12227, #1710, #1638, #13480, #4961, #14321, #7273, #1410, #14407, #10992, #13245, #3805, #13319, #12146, #6277, #9983, #562, #5273, #4122, #14722, #11143, #288, #11177, #14451, #5082, #3924, #13357, #14759, #1525, #7468, #2989, #13585, #14602, #5001, #1833, #11097, #2765, #519, #13516, #4084, #601, #8544, #7697, #446, #5236, #5311, #8787, #10023, #12184, #13441, #9718, #13281, #1603, #6460, #9867, #9944, #4157, #6236, #5155, #1750, #12264, #3845, #6316, #2916, #2847, #11030, #9795, #2683, #7382, #10868, #8859, #12102, #14681, #12411, #10952, #373, #14525, #4004, #8620 ),
 ( #1673, #7616, #8706, #7545, #6386, #12331, #13737, #11555, #11255, #4379, #9012, #6772, #827, #9166, #8075, #5459, #12725, #6839, #2136, #14910, #9088, #971, #15058, #748, #5678, #13809, #3364, #10176, #904, #14983, #13969, #10405, #12799, #7928, #8003, #6621, #5605, #3209, #6542, #15137, #676, #12646, #4532, #11329, #5532, #5382, #2060, #11488, #4452, #10319, #10251, #13893, #8936, #9242, #10096, #12490, #3290, #14832, #4231, #13664, #3065, #3136, #7776, #4307, #1907, #7850, #12567, #1979, #6695, #11409, #2287, #1274, #5978, #42, #2432, #15214, #10550, #1195, #14345, #10701, #11777, #4831, #9386, #4675, #12876, #9615, #6992, #9543, #117, #14269, #12955, #5897, #3668, #15283, #11633, #3598, #10619, #8452, #9468, #8370, #13100, #2515, #14194, #8299, #14116, #11848, #3517, #8146, #4752, #11708, #3748, #13027, #2205, #6912, #7210, #7127, #11930, #10776, #1354, #1051, #6058, #5758, #193, #4606, #1126, #10480, #7059, #4903, #9315, #5828, #14038, #3435, #8225, #2362, #1329, #4604, #1477, #11905, #6910, #6192, #5756, #1049, #7182, #9672, #3433, #10478, #12723, #13159, #170, #6033, #10908, #3362, #6111, #969, #326, #10753, #8144, #9589, #15212, #9312, #12874, #8506, #7346, #2568, #8073, #10824, #11553, #4877, #9757, #8426, #14036, #1406, #2285, #5039, #14485, #14317, #3721, #11631, #7269, #12797, #11983, #242, #4957, #14403, #10402, #3801, #13241, #3883, #2644, #12059, #2134, #6837, #5676, #2203, #15135, #4530, #9240, #13967, #11216, #4038, #12295, #636, #6349, #2720, #9979, #1706, #14870, #558, #1788, #4188, #7655, #5269, #14718, #5193, #2947, #9907, #14560, #6420, #3958, #10128, #4118, #8582, #13315, #6502, #8820, #14793, #1870, #13547, #7423, #11139, #12141, #12371, #6273, #2800, #709, #13476, #5340, #10057, #8665, #12452, #1559 ),
 ( #1634, #8894, #13626, #479, #3026, #10988, #7733, #11062, #6575, #2877, #11287, #404, #7504, #5413, #5113, #9828, #14641, #13396, #12223, #8743, #7577, #3396, #2091, #1083, #13769, #13925, #12676, #11666, #8105, #10510, #5636, #5714, #4340, #3244, #4266, #6801, #4486, #2169, #10350, #7956, #6871, #6651, #12830, #3098, #9273, #8968, #11517, #6727, #9196, #13842, #11587, #5790, #3164, #10433, #4564, #15171, #12600, #932, #13997, #12758, #7876, #2243, #15092, #13698, #2017, #3323, #8033, #7810, #6948, #12522, #1004, #1938, #9048, #11360, #787, #5492, #10211, #14945, #11440, #862, #5564, #10279, #15015, #4406, #9115, #8406, #14069, #2465, #12038, #10734, #11807, #3696, #8257, #3783, #1459, #3624, #7086, #9424, #1223, #14887, #14297, #13138, #13053, #148, #12908, #12984, #14223, #6167, #2548, #9500, #7249, #5934, #2389, #10577, #7326, #4712, #11964, #1387, #6088, #10658, #8327, #10805, #73, #9346, #1307, #7163, #15244, #11884, #220, #4935, #9652, #6010, #4858, #4785, #9569, #14383, #5858, #8489, #14150, #4636, #13220, #3472, #8184, #2623, #2322, #7021, #11735, #1155, #3550, #4020, #1851, #2861, #8562, #5097, #3009, #462, #13457, #6401, #1540, #14774, #306, #9961, #9738, #5020, #14467, #9810, #11046, #2700, #3939, #11196, #14698, #2782, #1619, #619, #3863, #5324, #13297, #14542, #8640, #13377, #4171, #6254, #7485, #7714, #13606, #14623, #7399, #10889, #11116, #12203, #538, #13532, #4101, #10037, #12123, #12430, #5173, #5251, #8875, #8802, #10970, #6331, #7561, #388, #9884, #8723, #6479, #12280, #2931, #1690, #7634, #12350, #1769, #5396, #6556, #691, #14850, #10111, #11268, #5000, #3764, #2605, #6071, #12263, #14364, #9866, #2915, #7615, #6385, #11096, #14524, #9717, #12330, #9794, #12101, #3923, #4082, #10788, #8619, #13280, #9943 ),
 ( #13356, #8543, #6315, #371, #8705, #204, #14449, #1672, #518, #5235, #3844, #2764, #14680, #14601, #287, #8786, #7467, #4917, #2682, #445, #12183, #13515, #9631, #8468, #1601, #7544, #6149, #5081, #13200, #11029, #5154, #4003, #13440, #2845, #7307, #12022, #1443, #10867, #7381, #1524, #6235, #10951, #13891, #12564, #13662, #5530, #10094, #5603, #3288, #5457, #8934, #8002, #1977, #6693, #1831, #2058, #10249, #825, #13583, #11407, #14830, #6459, #8857, #10174, #4155, #3134, #4229, #6619, #10317, #7774, #6770, #11176, #11485, #5309, #11253, #3063, #12488, #15056, #7695, #1905, #9164, #4450, #14908, #600, #1749, #14981, #11327, #4377, #9086, #13807, #902, #14757, #10022, #746, #3207, #2987, #7926, #12409, #4305, #9010, #6540, #674, #13735, #12644, #7848, #5380, #2181, #11457, #7751, #8911, #5729, #10295, #4205, #13639, #12695, #5580, #10371, #12774, #877, #3041, #12619, #10448, #15032, #1886, #13715, #11602, #9063, #6745, #4426, #10150, #8046, #12467, #3260, #6595, #11303, #724, #3114, #4355, #5430, #12541, #4502, #7973, #11383, #9210, #14884, #2033, #6667, #9136, #13785, #6814, #4281, #7827, #15109, #13940, #3338, #1952, #13862, #6885, #2109, #805, #1024, #11532, #8986, #5506, #946, #5650, #10228, #14962, #3183, #7895, #1325, #15258, #14166, #6106, #8272, #90, #13068, #1242, #3569, #7034, #3714, #13000, #9358, #8421, #8196, #3489, #9439, #11901, #5871, #12927, #15186, #4801, #2404, #7102, #13154, #5803, #8342, #3409, #2564, #11821, #10590, #5950, #2337, #11748, #9, #10748, #9585, #9517, #4580, #1170, #9287, #4728, #10673, #14238, #7265, #4873, #11681, #10525, #14012, #3640, #2483, #7178, #1399, #6027, #166, #4649, #14311, #11980, #8119, #1098, #12847, #2260, #6966, #14085, #14557, #13237, #12220, #8578, #401, #4114, #1555 ) ),
 .UNSPECIFIED., .T., .F., .T. ) 
 B_SPLINE_SURFACE_WITH_KNOTS ( ( 4, 3, 4 ),
 ( 3, 2, 2, 2, 2, 2, 2, 2, 2, 2, 2, 2, 2, 2, 2, 2, 2, 2, 2, 2, 2, 2, 2, 2, 2, 2, 2, 2, 2, 2, 2, 2, 2, 2, 2, 2, 2, 2, 2, 2, 2, 2, 2, 2, 2, 2, 2, 2, 2, 2, 2, 2, 2, 2, 2, 2, 2, 2, 2, 2, 2, 2, 2, 2, 2, 2, 2, 2, 2, 2, 2, 2, 2, 2, 2, 2, 2, 2, 2, 2, 2, 2, 2, 2, 2, 2, 2, 2, 2, 2, 2, 2, 2, 2, 2, 2, 2, 2, 2, 2, 2, 2, 2, 2, 2, 2, 2, 2, 2, 2, 2, 2, 2, 2, 2, 2, 2, 2, 2, 2, 3 ),
 ( 0.000000000000000000, 0.5000000000000000000, 1.000000000000000000 ),
 ( 0.000000000000000000, 0.008333333333333333218, 0.01666666666666666644, 0.02500000000000000139, 0.03333333333333333287, 0.04166666666666666435, 0.05000000000000000278, 0.05833333333333333426, 0.06666666666666666574, 0.07499999999999999722, 0.08333333333333332871, 0.09166666666666666019, 0.1000000000000000056, 0.1083333333333333370, 0.1166666666666666685, 0.1250000000000000000, 0.1333333333333333315, 0.1416666666666666630, 0.1499999999999999944, 0.1583333333333333259, 0.1666666666666666574, 0.1749999999999999889, 0.1833333333333333204, 0.1916666666666666519, 0.2000000000000000111, 0.2083333333333333426, 0.2166666666666666741, 0.2250000000000000056, 0.2333333333333333370, 0.2416666666666666685, 0.2500000000000000000, 0.2583333333333333037, 0.2666666666666666630, 0.2750000000000000222, 0.2833333333333333259, 0.2916666666666666852, 0.2999999999999999889, 0.3083333333333333481, 0.3166666666666666519, 0.3250000000000000111, 0.3333333333333333148, 0.3416666666666666741, 0.3499999999999999778, 0.3583333333333333370, 0.3666666666666666408, 0.3750000000000000000, 0.3833333333333333037, 0.3916666666666666630, 0.4000000000000000222, 0.4083333333333333259, 0.4166666666666666852, 0.4249999999999999889, 0.4333333333333333481, 0.4416666666666666519, 0.4500000000000000111, 0.4583333333333333148, 0.4666666666666666741, 0.4749999999999999778, 0.4833333333333333370, 0.4916666666666666408, 0.5000000000000000000, 0.5083333333333333037, 0.5166666666666666075, 0.5250000000000000222, 0.5333333333333333259, 0.5416666666666666297, 0.5500000000000000444, 0.5583333333333333481, 0.5666666666666666519, 0.5749999999999999556, 0.5833333333333333703, 0.5916666666666666741, 0.5999999999999999778, 0.6083333333333332815, 0.6166666666666666963, 0.6250000000000000000, 0.6333333333333333037, 0.6416666666666666075, 0.6500000000000000222, 0.6583333333333333259, 0.6666666666666666297, 0.6750000000000000444, 0.6833333333333333481, 0.6916666666666666519, 0.6999999999999999556, 0.7083333333333333703, 0.7166666666666666741, 0.7249999999999999778, 0.7333333333333332815, 0.7416666666666666963, 0.7500000000000000000, 0.7583333333333333037, 0.7666666666666666075, 0.7750000000000000222, 0.7833333333333333259, 0.7916666666666666297, 0.8000000000000000444, 0.8083333333333333481, 0.8166666666666666519, 0.8249999999999999556, 0.8333333333333333703, 0.8416666666666666741, 0.8499999999999999778, 0.8583333333333332815, 0.8666666666666666963, 0.8750000000000000000, 0.8833333333333333037, 0.8916666666666666075, 0.9000000000000000222, 0.9083333333333333259, 0.9166666666666666297, 0.9249999999999999334, 0.9333333333333333481, 0.9416666666666666519, 0.9499999999999999556, 0.9583333333333333703, 0.9666666666666666741, 0.9749999999999999778, 0.9833333333333332815, 0.9916666666666666963, 1.000000000000000000 ),
 .UNSPECIFIED. ) 
 GEOMETRIC_REPRESENTATION_ITEM ( )  RATIONAL_B_SPLINE_SURFACE ( (
 ( 1.000000000000000000, 0.9238795325112867385, 1.000000000000000000, 0.9238795325112867385, 1.000000000000000000, 0.9238795325112867385, 1.000000000000000000, 0.9238795325112867385, 1.000000000000000000, 0.9238795325112867385, 1.000000000000000000, 0.9238795325112867385, 1.000000000000000000, 0.9238795325112867385, 1.000000000000000000, 0.9238795325112867385, 1.000000000000000000, 0.9238795325112867385, 1.000000000000000000, 0.9238795325112867385, 1.000000000000000000, 0.9238795325112867385, 1.000000000000000000, 0.9238795325112867385, 1.000000000000000000, 0.9238795325112867385, 1.000000000000000000, 0.9238795325112867385, 1.000000000000000000, 0.9238795325112867385, 1.000000000000000000, 0.9238795325112867385, 1.000000000000000000, 0.9238795325112867385, 1.000000000000000000, 0.9238795325112867385, 1.000000000000000000, 0.9238795325112867385, 1.000000000000000000, 0.9238795325112867385, 1.000000000000000000, 0.9238795325112867385, 1.000000000000000000, 0.9238795325112867385, 1.000000000000000000, 0.9238795325112867385, 1.000000000000000000, 0.9238795325112867385, 1.000000000000000000, 0.9238795325112867385, 1.000000000000000000, 0.9238795325112867385, 1.000000000000000000, 0.9238795325112867385, 1.000000000000000000, 0.9238795325112867385, 1.000000000000000000, 0.9238795325112867385, 1.000000000000000000, 0.9238795325112867385, 1.000000000000000000, 0.9238795325112867385, 1.000000000000000000, 0.9238795325112867385, 1.000000000000000000, 0.9238795325112867385, 1.000000000000000000, 0.9238795325112867385, 1.000000000000000000, 0.9238795325112867385, 1.000000000000000000, 0.9238795325112867385, 1.000000000000000000, 0.9238795325112867385, 1.000000000000000000, 0.9238795325112867385, 1.000000000000000000, 0.9238795325112867385, 1.000000000000000000, 0.9238795325112867385, 1.000000000000000000, 0.9238795325112867385, 1.000000000000000000, 0.9238795325112867385, 1.000000000000000000, 0.9238795325112867385, 1.000000000000000000, 0.9238795325112867385, 1.000000000000000000, 0.9238795325112867385, 1.000000000000000000, 0.9238795325112867385, 1.000000000000000000, 0.9238795325112867385, 1.000000000000000000, 0.9238795325112867385, 1.000000000000000000, 0.9238795325112867385, 1.000000000000000000, 0.9238795325112867385, 1.000000000000000000, 0.9238795325112867385, 1.000000000000000000, 0.9238795325112867385, 1.000000000000000000, 0.9238795325112867385, 1.000000000000000000, 0.9238795325112867385, 1.000000000000000000, 0.9238795325112867385, 1.000000000000000000, 0.9238795325112867385, 1.000000000000000000, 0.9238795325112867385, 1.000000000000000000, 0.9238795325112867385, 1.000000000000000000, 0.9238795325112867385, 1.000000000000000000, 0.9238795325112867385, 1.000000000000000000, 0.9238795325112867385, 1.000000000000000000, 0.9238795325112867385, 1.000000000000000000, 0.9238795325112867385, 1.000000000000000000, 0.9238795325112867385, 1.000000000000000000, 0.9238795325112867385, 1.000000000000000000, 0.9238795325112867385, 1.000000000000000000, 0.9238795325112867385, 1.000000000000000000, 0.9238795325112867385, 1.000000000000000000, 0.9238795325112867385, 1.000000000000000000, 0.9238795325112867385, 1.000000000000000000, 0.9238795325112867385, 1.000000000000000000, 0.9238795325112867385, 1.000000000000000000, 0.9238795325112867385, 1.000000000000000000, 0.9238795325112867385, 1.000000000000000000, 0.9238795325112867385, 1.000000000000000000, 0.9238795325112867385, 1.000000000000000000, 0.9238795325112867385, 1.000000000000000000, 0.9238795325112867385, 1.000000000000000000, 0.9238795325112867385, 1.000000000000000000, 0.9238795325112867385, 1.000000000000000000, 0.9238795325112867385, 1.000000000000000000, 0.9238795325112867385, 1.000000000000000000, 0.9238795325112867385, 1.000000000000000000, 0.9238795325112867385, 1.000000000000000000, 0.9238795325112867385, 1.000000000000000000, 0.9238795325112867385, 1.000000000000000000, 0.9238795325112867385, 1.000000000000000000, 0.9238795325112867385, 1.000000000000000000, 0.9238795325112867385, 1.000000000000000000, 0.9238795325112867385, 1.000000000000000000, 0.9238795325112867385, 1.000000000000000000, 0.9238795325112867385, 1.000000000000000000, 0.9238795325112867385, 1.000000000000000000, 0.9238795325112867385, 1.000000000000000000, 0.9238795325112867385, 1.000000000000000000, 0.9238795325112867385, 1.000000000000000000, 0.9238795325112867385, 1.000000000000000000, 0.9238795325112867385, 1.000000000000000000, 0.9238795325112867385, 1.000000000000000000, 0.9238795325112867385, 1.000000000000000000, 0.9238795325112867385, 1.000000000000000000, 0.9238795325112867385, 1.000000000000000000, 0.9238795325112867385, 1.000000000000000000, 0.9238795325112867385, 1.000000000000000000, 0.9238795325112867385, 1.000000000000000000, 0.9238795325112867385, 1.000000000000000000, 0.9238795325112867385, 1.000000000000000000, 0.9238795325112867385, 1.000000000000000000, 0.9238795325112867385, 1.000000000000000000, 0.9238795325112867385, 1.000000000000000000, 0.9238795325112867385, 1.000000000000000000, 0.9238795325112867385, 1.000000000000000000, 0.9238795325112867385, 1.000000000000000000, 0.9238795325112867385, 1.000000000000000000, 0.9238795325112867385, 1.000000000000000000, 0.9238795325112867385, 1.000000000000000000, 0.9238795325112867385, 1.000000000000000000, 0.9238795325112867385, 1.000000000000000000, 0.9238795325112867385, 1.000000000000000000, 0.9238795325112867385, 1.000000000000000000),
 ( 0.3333333333333333703, 0.3079598441704289313, 0.3333333333333333703, 0.3079598441704289313, 0.3333333333333333703, 0.3079598441704289313, 0.3333333333333333703, 0.3079598441704289313, 0.3333333333333333703, 0.3079598441704289313, 0.3333333333333333703, 0.3079598441704289313, 0.3333333333333333703, 0.3079598441704289313, 0.3333333333333333703, 0.3079598441704289313, 0.3333333333333333703, 0.3079598441704289313, 0.3333333333333333703, 0.3079598441704289313, 0.3333333333333333703, 0.3079598441704289313, 0.3333333333333333703, 0.3079598441704289313, 0.3333333333333333703, 0.3079598441704289313, 0.3333333333333333703, 0.3079598441704289313, 0.3333333333333333703, 0.3079598441704289313, 0.3333333333333333703, 0.3079598441704289313, 0.3333333333333333703, 0.3079598441704289313, 0.3333333333333333703, 0.3079598441704289313, 0.3333333333333333703, 0.3079598441704289313, 0.3333333333333333703, 0.3079598441704289313, 0.3333333333333333703, 0.3079598441704289313, 0.3333333333333333703, 0.3079598441704289313, 0.3333333333333333703, 0.3079598441704289313, 0.3333333333333333703, 0.3079598441704289313, 0.3333333333333333703, 0.3079598441704289313, 0.3333333333333333703, 0.3079598441704289313, 0.3333333333333333703, 0.3079598441704289313, 0.3333333333333333703, 0.3079598441704289313, 0.3333333333333333703, 0.3079598441704289313, 0.3333333333333333703, 0.3079598441704289313, 0.3333333333333333703, 0.3079598441704289313, 0.3333333333333333703, 0.3079598441704289313, 0.3333333333333333703, 0.3079598441704289313, 0.3333333333333333703, 0.3079598441704289313, 0.3333333333333333703, 0.3079598441704289313, 0.3333333333333333703, 0.3079598441704289313, 0.3333333333333333703, 0.3079598441704289313, 0.3333333333333333703, 0.3079598441704289313, 0.3333333333333333703, 0.3079598441704289313, 0.3333333333333333703, 0.3079598441704289313, 0.3333333333333333703, 0.3079598441704289313, 0.3333333333333333703, 0.3079598441704289313, 0.3333333333333333703, 0.3079598441704289313, 0.3333333333333333703, 0.3079598441704289313, 0.3333333333333333703, 0.3079598441704289313, 0.3333333333333333703, 0.3079598441704289313, 0.3333333333333333703, 0.3079598441704289313, 0.3333333333333333703, 0.3079598441704289313, 0.3333333333333333703, 0.3079598441704289313, 0.3333333333333333703, 0.3079598441704289313, 0.3333333333333333703, 0.3079598441704289313, 0.3333333333333333703, 0.3079598441704289313, 0.3333333333333333703, 0.3079598441704289313, 0.3333333333333333703, 0.3079598441704289313, 0.3333333333333333703, 0.3079598441704289313, 0.3333333333333333703, 0.3079598441704289313, 0.3333333333333333703, 0.3079598441704289313, 0.3333333333333333703, 0.3079598441704289313, 0.3333333333333333703, 0.3079598441704289313, 0.3333333333333333703, 0.3079598441704289313, 0.3333333333333333703, 0.3079598441704289313, 0.3333333333333333703, 0.3079598441704289313, 0.3333333333333333703, 0.3079598441704289313, 0.3333333333333333703, 0.3079598441704289313, 0.3333333333333333703, 0.3079598441704289313, 0.3333333333333333703, 0.3079598441704289313, 0.3333333333333333703, 0.3079598441704289313, 0.3333333333333333703, 0.3079598441704289313, 0.3333333333333333703, 0.3079598441704289313, 0.3333333333333333703, 0.3079598441704289313, 0.3333333333333333703, 0.3079598441704289313, 0.3333333333333333703, 0.3079598441704289313, 0.3333333333333333703, 0.3079598441704289313, 0.3333333333333333703, 0.3079598441704289313, 0.3333333333333333703, 0.3079598441704289313, 0.3333333333333333703, 0.3079598441704289313, 0.3333333333333333703, 0.3079598441704289313, 0.3333333333333333703, 0.3079598441704289313, 0.3333333333333333703, 0.3079598441704289313, 0.3333333333333333703, 0.3079598441704289313, 0.3333333333333333703, 0.3079598441704289313, 0.3333333333333333703, 0.3079598441704289313, 0.3333333333333333703, 0.3079598441704289313, 0.3333333333333333703, 0.3079598441704289313, 0.3333333333333333703, 0.3079598441704289313, 0.3333333333333333703, 0.3079598441704289313, 0.3333333333333333703, 0.3079598441704289313, 0.3333333333333333703, 0.3079598441704289313, 0.3333333333333333703, 0.3079598441704289313, 0.3333333333333333703, 0.3079598441704289313, 0.3333333333333333703, 0.3079598441704289313, 0.3333333333333333703, 0.3079598441704289313, 0.3333333333333333703, 0.3079598441704289313, 0.3333333333333333703, 0.3079598441704289313, 0.3333333333333333703, 0.3079598441704289313, 0.3333333333333333703, 0.3079598441704289313, 0.3333333333333333703, 0.3079598441704289313, 0.3333333333333333703, 0.3079598441704289313, 0.3333333333333333703, 0.3079598441704289313, 0.3333333333333333703, 0.3079598441704289313, 0.3333333333333333703, 0.3079598441704289313, 0.3333333333333333703, 0.3079598441704289313, 0.3333333333333333703, 0.3079598441704289313, 0.3333333333333333703, 0.3079598441704289313, 0.3333333333333333703, 0.3079598441704289313, 0.3333333333333333703, 0.3079598441704289313, 0.3333333333333333703, 0.3079598441704289313, 0.3333333333333333703, 0.3079598441704289313, 0.3333333333333333703, 0.3079598441704289313, 0.3333333333333333703, 0.3079598441704289313, 0.3333333333333333703, 0.3079598441704289313, 0.3333333333333333703, 0.3079598441704289313, 0.3333333333333333703, 0.3079598441704289313, 0.3333333333333333703, 0.3079598441704289313, 0.3333333333333333703, 0.3079598441704289313, 0.3333333333333333703, 0.3079598441704289313, 0.3333333333333333703, 0.3079598441704289313, 0.3333333333333333703, 0.3079598441704289313, 0.3333333333333333703, 0.3079598441704289313, 0.3333333333333333703, 0.3079598441704289313, 0.3333333333333333703),
 ( 0.3333333333333333703, 0.3079598441704289313, 0.3333333333333333703, 0.3079598441704289313, 0.3333333333333333703, 0.3079598441704289313, 0.3333333333333333703, 0.3079598441704289313, 0.3333333333333333703, 0.3079598441704289313, 0.3333333333333333703, 0.3079598441704289313, 0.3333333333333333703, 0.3079598441704289313, 0.3333333333333333703, 0.3079598441704289313, 0.3333333333333333703, 0.3079598441704289313, 0.3333333333333333703, 0.3079598441704289313, 0.3333333333333333703, 0.3079598441704289313, 0.3333333333333333703, 0.3079598441704289313, 0.3333333333333333703, 0.3079598441704289313, 0.3333333333333333703, 0.3079598441704289313, 0.3333333333333333703, 0.3079598441704289313, 0.3333333333333333703, 0.3079598441704289313, 0.3333333333333333703, 0.3079598441704289313, 0.3333333333333333703, 0.3079598441704289313, 0.3333333333333333703, 0.3079598441704289313, 0.3333333333333333703, 0.3079598441704289313, 0.3333333333333333703, 0.3079598441704289313, 0.3333333333333333703, 0.3079598441704289313, 0.3333333333333333703, 0.3079598441704289313, 0.3333333333333333703, 0.3079598441704289313, 0.3333333333333333703, 0.3079598441704289313, 0.3333333333333333703, 0.3079598441704289313, 0.3333333333333333703, 0.3079598441704289313, 0.3333333333333333703, 0.3079598441704289313, 0.3333333333333333703, 0.3079598441704289313, 0.3333333333333333703, 0.3079598441704289313, 0.3333333333333333703, 0.3079598441704289313, 0.3333333333333333703, 0.3079598441704289313, 0.3333333333333333703, 0.3079598441704289313, 0.3333333333333333703, 0.3079598441704289313, 0.3333333333333333703, 0.3079598441704289313, 0.3333333333333333703, 0.3079598441704289313, 0.3333333333333333703, 0.3079598441704289313, 0.3333333333333333703, 0.3079598441704289313, 0.3333333333333333703, 0.3079598441704289313, 0.3333333333333333703, 0.3079598441704289313, 0.3333333333333333703, 0.3079598441704289313, 0.3333333333333333703, 0.3079598441704289313, 0.3333333333333333703, 0.3079598441704289313, 0.3333333333333333703, 0.3079598441704289313, 0.3333333333333333703, 0.3079598441704289313, 0.3333333333333333703, 0.3079598441704289313, 0.3333333333333333703, 0.3079598441704289313, 0.3333333333333333703, 0.3079598441704289313, 0.3333333333333333703, 0.3079598441704289313, 0.3333333333333333703, 0.3079598441704289313, 0.3333333333333333703, 0.3079598441704289313, 0.3333333333333333703, 0.3079598441704289313, 0.3333333333333333703, 0.3079598441704289313, 0.3333333333333333703, 0.3079598441704289313, 0.3333333333333333703, 0.3079598441704289313, 0.3333333333333333703, 0.3079598441704289313, 0.3333333333333333703, 0.3079598441704289313, 0.3333333333333333703, 0.3079598441704289313, 0.3333333333333333703, 0.3079598441704289313, 0.3333333333333333703, 0.3079598441704289313, 0.3333333333333333703, 0.3079598441704289313, 0.3333333333333333703, 0.3079598441704289313, 0.3333333333333333703, 0.3079598441704289313, 0.3333333333333333703, 0.3079598441704289313, 0.3333333333333333703, 0.3079598441704289313, 0.3333333333333333703, 0.3079598441704289313, 0.3333333333333333703, 0.3079598441704289313, 0.3333333333333333703, 0.3079598441704289313, 0.3333333333333333703, 0.3079598441704289313, 0.3333333333333333703, 0.3079598441704289313, 0.3333333333333333703, 0.3079598441704289313, 0.3333333333333333703, 0.3079598441704289313, 0.3333333333333333703, 0.3079598441704289313, 0.3333333333333333703, 0.3079598441704289313, 0.3333333333333333703, 0.3079598441704289313, 0.3333333333333333703, 0.3079598441704289313, 0.3333333333333333703, 0.3079598441704289313, 0.3333333333333333703, 0.3079598441704289313, 0.3333333333333333703, 0.3079598441704289313, 0.3333333333333333703, 0.3079598441704289313, 0.3333333333333333703, 0.3079598441704289313, 0.3333333333333333703, 0.3079598441704289313, 0.3333333333333333703, 0.3079598441704289313, 0.3333333333333333703, 0.3079598441704289313, 0.3333333333333333703, 0.3079598441704289313, 0.3333333333333333703, 0.3079598441704289313, 0.3333333333333333703, 0.3079598441704289313, 0.3333333333333333703, 0.3079598441704289313, 0.3333333333333333703, 0.3079598441704289313, 0.3333333333333333703, 0.3079598441704289313, 0.3333333333333333703, 0.3079598441704289313, 0.3333333333333333703, 0.3079598441704289313, 0.3333333333333333703, 0.3079598441704289313, 0.3333333333333333703, 0.3079598441704289313, 0.3333333333333333703, 0.3079598441704289313, 0.3333333333333333703, 0.3079598441704289313, 0.3333333333333333703, 0.3079598441704289313, 0.3333333333333333703, 0.3079598441704289313, 0.3333333333333333703, 0.3079598441704289313, 0.3333333333333333703, 0.3079598441704289313, 0.3333333333333333703, 0.3079598441704289313, 0.3333333333333333703, 0.3079598441704289313, 0.3333333333333333703, 0.3079598441704289313, 0.3333333333333333703, 0.3079598441704289313, 0.3333333333333333703, 0.3079598441704289313, 0.3333333333333333703, 0.3079598441704289313, 0.3333333333333333703, 0.3079598441704289313, 0.3333333333333333703, 0.3079598441704289313, 0.3333333333333333703, 0.3079598441704289313, 0.3333333333333333703, 0.3079598441704289313, 0.3333333333333333703, 0.3079598441704289313, 0.3333333333333333703, 0.3079598441704289313, 0.3333333333333333703, 0.3079598441704289313, 0.3333333333333333703, 0.3079598441704289313, 0.3333333333333333703, 0.3079598441704289313, 0.3333333333333333703, 0.3079598441704289313, 0.3333333333333333703, 0.3079598441704289313, 0.3333333333333333703, 0.3079598441704289313, 0.3333333333333333703, 0.3079598441704289313, 0.3333333333333333703, 0.3079598441704289313, 0.3333333333333333703),
 ( 1.000000000000000000, 0.9238795325112867385, 1.000000000000000000, 0.9238795325112867385, 1.000000000000000000, 0.9238795325112867385, 1.000000000000000000, 0.9238795325112867385, 1.000000000000000000, 0.9238795325112867385, 1.000000000000000000, 0.9238795325112867385, 1.000000000000000000, 0.9238795325112867385, 1.000000000000000000, 0.9238795325112867385, 1.000000000000000000, 0.9238795325112867385, 1.000000000000000000, 0.9238795325112867385, 1.000000000000000000, 0.9238795325112867385, 1.000000000000000000, 0.9238795325112867385, 1.000000000000000000, 0.9238795325112867385, 1.000000000000000000, 0.9238795325112867385, 1.000000000000000000, 0.9238795325112867385, 1.000000000000000000, 0.9238795325112867385, 1.000000000000000000, 0.9238795325112867385, 1.000000000000000000, 0.9238795325112867385, 1.000000000000000000, 0.9238795325112867385, 1.000000000000000000, 0.9238795325112867385, 1.000000000000000000, 0.9238795325112867385, 1.000000000000000000, 0.9238795325112867385, 1.000000000000000000, 0.9238795325112867385, 1.000000000000000000, 0.9238795325112867385, 1.000000000000000000, 0.9238795325112867385, 1.000000000000000000, 0.9238795325112867385, 1.000000000000000000, 0.9238795325112867385, 1.000000000000000000, 0.9238795325112867385, 1.000000000000000000, 0.9238795325112867385, 1.000000000000000000, 0.9238795325112867385, 1.000000000000000000, 0.9238795325112867385, 1.000000000000000000, 0.9238795325112867385, 1.000000000000000000, 0.9238795325112867385, 1.000000000000000000, 0.9238795325112867385, 1.000000000000000000, 0.9238795325112867385, 1.000000000000000000, 0.9238795325112867385, 1.000000000000000000, 0.9238795325112867385, 1.000000000000000000, 0.9238795325112867385, 1.000000000000000000, 0.9238795325112867385, 1.000000000000000000, 0.9238795325112867385, 1.000000000000000000, 0.9238795325112867385, 1.000000000000000000, 0.9238795325112867385, 1.000000000000000000, 0.9238795325112867385, 1.000000000000000000, 0.9238795325112867385, 1.000000000000000000, 0.9238795325112867385, 1.000000000000000000, 0.9238795325112867385, 1.000000000000000000, 0.9238795325112867385, 1.000000000000000000, 0.9238795325112867385, 1.000000000000000000, 0.9238795325112867385, 1.000000000000000000, 0.9238795325112867385, 1.000000000000000000, 0.9238795325112867385, 1.000000000000000000, 0.9238795325112867385, 1.000000000000000000, 0.9238795325112867385, 1.000000000000000000, 0.9238795325112867385, 1.000000000000000000, 0.9238795325112867385, 1.000000000000000000, 0.9238795325112867385, 1.000000000000000000, 0.9238795325112867385, 1.000000000000000000, 0.9238795325112867385, 1.000000000000000000, 0.9238795325112867385, 1.000000000000000000, 0.9238795325112867385, 1.000000000000000000, 0.9238795325112867385, 1.000000000000000000, 0.9238795325112867385, 1.000000000000000000, 0.9238795325112867385, 1.000000000000000000, 0.9238795325112867385, 1.000000000000000000, 0.9238795325112867385, 1.000000000000000000, 0.9238795325112867385, 1.000000000000000000, 0.9238795325112867385, 1.000000000000000000, 0.9238795325112867385, 1.000000000000000000, 0.9238795325112867385, 1.000000000000000000, 0.9238795325112867385, 1.000000000000000000, 0.9238795325112867385, 1.000000000000000000, 0.9238795325112867385, 1.000000000000000000, 0.9238795325112867385, 1.000000000000000000, 0.9238795325112867385, 1.000000000000000000, 0.9238795325112867385, 1.000000000000000000, 0.9238795325112867385, 1.000000000000000000, 0.9238795325112867385, 1.000000000000000000, 0.9238795325112867385, 1.000000000000000000, 0.9238795325112867385, 1.000000000000000000, 0.9238795325112867385, 1.000000000000000000, 0.9238795325112867385, 1.000000000000000000, 0.9238795325112867385, 1.000000000000000000, 0.9238795325112867385, 1.000000000000000000, 0.9238795325112867385, 1.000000000000000000, 0.9238795325112867385, 1.000000000000000000, 0.9238795325112867385, 1.000000000000000000, 0.9238795325112867385, 1.000000000000000000, 0.9238795325112867385, 1.000000000000000000, 0.9238795325112867385, 1.000000000000000000, 0.9238795325112867385, 1.000000000000000000, 0.9238795325112867385, 1.000000000000000000, 0.9238795325112867385, 1.000000000000000000, 0.9238795325112867385, 1.000000000000000000, 0.9238795325112867385, 1.000000000000000000, 0.9238795325112867385, 1.000000000000000000, 0.9238795325112867385, 1.000000000000000000, 0.9238795325112867385, 1.000000000000000000, 0.9238795325112867385, 1.000000000000000000, 0.9238795325112867385, 1.000000000000000000, 0.9238795325112867385, 1.000000000000000000, 0.9238795325112867385, 1.000000000000000000, 0.9238795325112867385, 1.000000000000000000, 0.9238795325112867385, 1.000000000000000000, 0.9238795325112867385, 1.000000000000000000, 0.9238795325112867385, 1.000000000000000000, 0.9238795325112867385, 1.000000000000000000, 0.9238795325112867385, 1.000000000000000000, 0.9238795325112867385, 1.000000000000000000, 0.9238795325112867385, 1.000000000000000000, 0.9238795325112867385, 1.000000000000000000, 0.9238795325112867385, 1.000000000000000000, 0.9238795325112867385, 1.000000000000000000, 0.9238795325112867385, 1.000000000000000000, 0.9238795325112867385, 1.000000000000000000, 0.9238795325112867385, 1.000000000000000000, 0.9238795325112867385, 1.000000000000000000, 0.9238795325112867385, 1.000000000000000000, 0.9238795325112867385, 1.000000000000000000, 0.9238795325112867385, 1.000000000000000000, 0.9238795325112867385, 1.000000000000000000),
 ( 0.3333333333333333703, 0.3079598441704289313, 0.3333333333333333703, 0.3079598441704289313, 0.3333333333333333703, 0.3079598441704289313, 0.3333333333333333703, 0.3079598441704289313, 0.3333333333333333703, 0.3079598441704289313, 0.3333333333333333703, 0.3079598441704289313, 0.3333333333333333703, 0.3079598441704289313, 0.3333333333333333703, 0.3079598441704289313, 0.3333333333333333703, 0.3079598441704289313, 0.3333333333333333703, 0.3079598441704289313, 0.3333333333333333703, 0.3079598441704289313, 0.3333333333333333703, 0.3079598441704289313, 0.3333333333333333703, 0.3079598441704289313, 0.3333333333333333703, 0.3079598441704289313, 0.3333333333333333703, 0.3079598441704289313, 0.3333333333333333703, 0.3079598441704289313, 0.3333333333333333703, 0.3079598441704289313, 0.3333333333333333703, 0.3079598441704289313, 0.3333333333333333703, 0.3079598441704289313, 0.3333333333333333703, 0.3079598441704289313, 0.3333333333333333703, 0.3079598441704289313, 0.3333333333333333703, 0.3079598441704289313, 0.3333333333333333703, 0.3079598441704289313, 0.3333333333333333703, 0.3079598441704289313, 0.3333333333333333703, 0.3079598441704289313, 0.3333333333333333703, 0.3079598441704289313, 0.3333333333333333703, 0.3079598441704289313, 0.3333333333333333703, 0.3079598441704289313, 0.3333333333333333703, 0.3079598441704289313, 0.3333333333333333703, 0.3079598441704289313, 0.3333333333333333703, 0.3079598441704289313, 0.3333333333333333703, 0.3079598441704289313, 0.3333333333333333703, 0.3079598441704289313, 0.3333333333333333703, 0.3079598441704289313, 0.3333333333333333703, 0.3079598441704289313, 0.3333333333333333703, 0.3079598441704289313, 0.3333333333333333703, 0.3079598441704289313, 0.3333333333333333703, 0.3079598441704289313, 0.3333333333333333703, 0.3079598441704289313, 0.3333333333333333703, 0.3079598441704289313, 0.3333333333333333703, 0.3079598441704289313, 0.3333333333333333703, 0.3079598441704289313, 0.3333333333333333703, 0.3079598441704289313, 0.3333333333333333703, 0.3079598441704289313, 0.3333333333333333703, 0.3079598441704289313, 0.3333333333333333703, 0.3079598441704289313, 0.3333333333333333703, 0.3079598441704289313, 0.3333333333333333703, 0.3079598441704289313, 0.3333333333333333703, 0.3079598441704289313, 0.3333333333333333703, 0.3079598441704289313, 0.3333333333333333703, 0.3079598441704289313, 0.3333333333333333703, 0.3079598441704289313, 0.3333333333333333703, 0.3079598441704289313, 0.3333333333333333703, 0.3079598441704289313, 0.3333333333333333703, 0.3079598441704289313, 0.3333333333333333703, 0.3079598441704289313, 0.3333333333333333703, 0.3079598441704289313, 0.3333333333333333703, 0.3079598441704289313, 0.3333333333333333703, 0.3079598441704289313, 0.3333333333333333703, 0.3079598441704289313, 0.3333333333333333703, 0.3079598441704289313, 0.3333333333333333703, 0.3079598441704289313, 0.3333333333333333703, 0.3079598441704289313, 0.3333333333333333703, 0.3079598441704289313, 0.3333333333333333703, 0.3079598441704289313, 0.3333333333333333703, 0.3079598441704289313, 0.3333333333333333703, 0.3079598441704289313, 0.3333333333333333703, 0.3079598441704289313, 0.3333333333333333703, 0.3079598441704289313, 0.3333333333333333703, 0.3079598441704289313, 0.3333333333333333703, 0.3079598441704289313, 0.3333333333333333703, 0.3079598441704289313, 0.3333333333333333703, 0.3079598441704289313, 0.3333333333333333703, 0.3079598441704289313, 0.3333333333333333703, 0.3079598441704289313, 0.3333333333333333703, 0.3079598441704289313, 0.3333333333333333703, 0.3079598441704289313, 0.3333333333333333703, 0.3079598441704289313, 0.3333333333333333703, 0.3079598441704289313, 0.3333333333333333703, 0.3079598441704289313, 0.3333333333333333703, 0.3079598441704289313, 0.3333333333333333703, 0.3079598441704289313, 0.3333333333333333703, 0.3079598441704289313, 0.3333333333333333703, 0.3079598441704289313, 0.3333333333333333703, 0.3079598441704289313, 0.3333333333333333703, 0.3079598441704289313, 0.3333333333333333703, 0.3079598441704289313, 0.3333333333333333703, 0.3079598441704289313, 0.3333333333333333703, 0.3079598441704289313, 0.3333333333333333703, 0.3079598441704289313, 0.3333333333333333703, 0.3079598441704289313, 0.3333333333333333703, 0.3079598441704289313, 0.3333333333333333703, 0.3079598441704289313, 0.3333333333333333703, 0.3079598441704289313, 0.3333333333333333703, 0.3079598441704289313, 0.3333333333333333703, 0.3079598441704289313, 0.3333333333333333703, 0.3079598441704289313, 0.3333333333333333703, 0.3079598441704289313, 0.3333333333333333703, 0.3079598441704289313, 0.3333333333333333703, 0.3079598441704289313, 0.3333333333333333703, 0.3079598441704289313, 0.3333333333333333703, 0.3079598441704289313, 0.3333333333333333703, 0.3079598441704289313, 0.3333333333333333703, 0.3079598441704289313, 0.3333333333333333703, 0.3079598441704289313, 0.3333333333333333703, 0.3079598441704289313, 0.3333333333333333703, 0.3079598441704289313, 0.3333333333333333703, 0.3079598441704289313, 0.3333333333333333703, 0.3079598441704289313, 0.3333333333333333703, 0.3079598441704289313, 0.3333333333333333703, 0.3079598441704289313, 0.3333333333333333703, 0.3079598441704289313, 0.3333333333333333703, 0.3079598441704289313, 0.3333333333333333703, 0.3079598441704289313, 0.3333333333333333703, 0.3079598441704289313, 0.3333333333333333703, 0.3079598441704289313, 0.3333333333333333703, 0.3079598441704289313, 0.3333333333333333703, 0.3079598441704289313, 0.3333333333333333703, 0.3079598441704289313, 0.3333333333333333703, 0.3079598441704289313, 0.3333333333333333703),
 ( 0.3333333333333333703, 0.3079598441704289313, 0.3333333333333333703, 0.3079598441704289313, 0.3333333333333333703, 0.3079598441704289313, 0.3333333333333333703, 0.3079598441704289313, 0.3333333333333333703, 0.3079598441704289313, 0.3333333333333333703, 0.3079598441704289313, 0.3333333333333333703, 0.3079598441704289313, 0.3333333333333333703, 0.3079598441704289313, 0.3333333333333333703, 0.3079598441704289313, 0.3333333333333333703, 0.3079598441704289313, 0.3333333333333333703, 0.3079598441704289313, 0.3333333333333333703, 0.3079598441704289313, 0.3333333333333333703, 0.3079598441704289313, 0.3333333333333333703, 0.3079598441704289313, 0.3333333333333333703, 0.3079598441704289313, 0.3333333333333333703, 0.3079598441704289313, 0.3333333333333333703, 0.3079598441704289313, 0.3333333333333333703, 0.3079598441704289313, 0.3333333333333333703, 0.3079598441704289313, 0.3333333333333333703, 0.3079598441704289313, 0.3333333333333333703, 0.3079598441704289313, 0.3333333333333333703, 0.3079598441704289313, 0.3333333333333333703, 0.3079598441704289313, 0.3333333333333333703, 0.3079598441704289313, 0.3333333333333333703, 0.3079598441704289313, 0.3333333333333333703, 0.3079598441704289313, 0.3333333333333333703, 0.3079598441704289313, 0.3333333333333333703, 0.3079598441704289313, 0.3333333333333333703, 0.3079598441704289313, 0.3333333333333333703, 0.3079598441704289313, 0.3333333333333333703, 0.3079598441704289313, 0.3333333333333333703, 0.3079598441704289313, 0.3333333333333333703, 0.3079598441704289313, 0.3333333333333333703, 0.3079598441704289313, 0.3333333333333333703, 0.3079598441704289313, 0.3333333333333333703, 0.3079598441704289313, 0.3333333333333333703, 0.3079598441704289313, 0.3333333333333333703, 0.3079598441704289313, 0.3333333333333333703, 0.3079598441704289313, 0.3333333333333333703, 0.3079598441704289313, 0.3333333333333333703, 0.3079598441704289313, 0.3333333333333333703, 0.3079598441704289313, 0.3333333333333333703, 0.3079598441704289313, 0.3333333333333333703, 0.3079598441704289313, 0.3333333333333333703, 0.3079598441704289313, 0.3333333333333333703, 0.3079598441704289313, 0.3333333333333333703, 0.3079598441704289313, 0.3333333333333333703, 0.3079598441704289313, 0.3333333333333333703, 0.3079598441704289313, 0.3333333333333333703, 0.3079598441704289313, 0.3333333333333333703, 0.3079598441704289313, 0.3333333333333333703, 0.3079598441704289313, 0.3333333333333333703, 0.3079598441704289313, 0.3333333333333333703, 0.3079598441704289313, 0.3333333333333333703, 0.3079598441704289313, 0.3333333333333333703, 0.3079598441704289313, 0.3333333333333333703, 0.3079598441704289313, 0.3333333333333333703, 0.3079598441704289313, 0.3333333333333333703, 0.3079598441704289313, 0.3333333333333333703, 0.3079598441704289313, 0.3333333333333333703, 0.3079598441704289313, 0.3333333333333333703, 0.3079598441704289313, 0.3333333333333333703, 0.3079598441704289313, 0.3333333333333333703, 0.3079598441704289313, 0.3333333333333333703, 0.3079598441704289313, 0.3333333333333333703, 0.3079598441704289313, 0.3333333333333333703, 0.3079598441704289313, 0.3333333333333333703, 0.3079598441704289313, 0.3333333333333333703, 0.3079598441704289313, 0.3333333333333333703, 0.3079598441704289313, 0.3333333333333333703, 0.3079598441704289313, 0.3333333333333333703, 0.3079598441704289313, 0.3333333333333333703, 0.3079598441704289313, 0.3333333333333333703, 0.3079598441704289313, 0.3333333333333333703, 0.3079598441704289313, 0.3333333333333333703, 0.3079598441704289313, 0.3333333333333333703, 0.3079598441704289313, 0.3333333333333333703, 0.3079598441704289313, 0.3333333333333333703, 0.3079598441704289313, 0.3333333333333333703, 0.3079598441704289313, 0.3333333333333333703, 0.3079598441704289313, 0.3333333333333333703, 0.3079598441704289313, 0.3333333333333333703, 0.3079598441704289313, 0.3333333333333333703, 0.3079598441704289313, 0.3333333333333333703, 0.3079598441704289313, 0.3333333333333333703, 0.3079598441704289313, 0.3333333333333333703, 0.3079598441704289313, 0.3333333333333333703, 0.3079598441704289313, 0.3333333333333333703, 0.3079598441704289313, 0.3333333333333333703, 0.3079598441704289313, 0.3333333333333333703, 0.3079598441704289313, 0.3333333333333333703, 0.3079598441704289313, 0.3333333333333333703, 0.3079598441704289313, 0.3333333333333333703, 0.3079598441704289313, 0.3333333333333333703, 0.3079598441704289313, 0.3333333333333333703, 0.3079598441704289313, 0.3333333333333333703, 0.3079598441704289313, 0.3333333333333333703, 0.3079598441704289313, 0.3333333333333333703, 0.3079598441704289313, 0.3333333333333333703, 0.3079598441704289313, 0.3333333333333333703, 0.3079598441704289313, 0.3333333333333333703, 0.3079598441704289313, 0.3333333333333333703, 0.3079598441704289313, 0.3333333333333333703, 0.3079598441704289313, 0.3333333333333333703, 0.3079598441704289313, 0.3333333333333333703, 0.3079598441704289313, 0.3333333333333333703, 0.3079598441704289313, 0.3333333333333333703, 0.3079598441704289313, 0.3333333333333333703, 0.3079598441704289313, 0.3333333333333333703, 0.3079598441704289313, 0.3333333333333333703, 0.3079598441704289313, 0.3333333333333333703, 0.3079598441704289313, 0.3333333333333333703, 0.3079598441704289313, 0.3333333333333333703, 0.3079598441704289313, 0.3333333333333333703, 0.3079598441704289313, 0.3333333333333333703, 0.3079598441704289313, 0.3333333333333333703, 0.3079598441704289313, 0.3333333333333333703, 0.3079598441704289313, 0.3333333333333333703, 0.3079598441704289313, 0.3333333333333333703, 0.3079598441704289313, 0.3333333333333333703),
 ( 1.000000000000000000, 0.9238795325112867385, 1.000000000000000000, 0.9238795325112867385, 1.000000000000000000, 0.9238795325112867385, 1.000000000000000000, 0.9238795325112867385, 1.000000000000000000, 0.9238795325112867385, 1.000000000000000000, 0.9238795325112867385, 1.000000000000000000, 0.9238795325112867385, 1.000000000000000000, 0.9238795325112867385, 1.000000000000000000, 0.9238795325112867385, 1.000000000000000000, 0.9238795325112867385, 1.000000000000000000, 0.9238795325112867385, 1.000000000000000000, 0.9238795325112867385, 1.000000000000000000, 0.9238795325112867385, 1.000000000000000000, 0.9238795325112867385, 1.000000000000000000, 0.9238795325112867385, 1.000000000000000000, 0.9238795325112867385, 1.000000000000000000, 0.9238795325112867385, 1.000000000000000000, 0.9238795325112867385, 1.000000000000000000, 0.9238795325112867385, 1.000000000000000000, 0.9238795325112867385, 1.000000000000000000, 0.9238795325112867385, 1.000000000000000000, 0.9238795325112867385, 1.000000000000000000, 0.9238795325112867385, 1.000000000000000000, 0.9238795325112867385, 1.000000000000000000, 0.9238795325112867385, 1.000000000000000000, 0.9238795325112867385, 1.000000000000000000, 0.9238795325112867385, 1.000000000000000000, 0.9238795325112867385, 1.000000000000000000, 0.9238795325112867385, 1.000000000000000000, 0.9238795325112867385, 1.000000000000000000, 0.9238795325112867385, 1.000000000000000000, 0.9238795325112867385, 1.000000000000000000, 0.9238795325112867385, 1.000000000000000000, 0.9238795325112867385, 1.000000000000000000, 0.9238795325112867385, 1.000000000000000000, 0.9238795325112867385, 1.000000000000000000, 0.9238795325112867385, 1.000000000000000000, 0.9238795325112867385, 1.000000000000000000, 0.9238795325112867385, 1.000000000000000000, 0.9238795325112867385, 1.000000000000000000, 0.9238795325112867385, 1.000000000000000000, 0.9238795325112867385, 1.000000000000000000, 0.9238795325112867385, 1.000000000000000000, 0.9238795325112867385, 1.000000000000000000, 0.9238795325112867385, 1.000000000000000000, 0.9238795325112867385, 1.000000000000000000, 0.9238795325112867385, 1.000000000000000000, 0.9238795325112867385, 1.000000000000000000, 0.9238795325112867385, 1.000000000000000000, 0.9238795325112867385, 1.000000000000000000, 0.9238795325112867385, 1.000000000000000000, 0.9238795325112867385, 1.000000000000000000, 0.9238795325112867385, 1.000000000000000000, 0.9238795325112867385, 1.000000000000000000, 0.9238795325112867385, 1.000000000000000000, 0.9238795325112867385, 1.000000000000000000, 0.9238795325112867385, 1.000000000000000000, 0.9238795325112867385, 1.000000000000000000, 0.9238795325112867385, 1.000000000000000000, 0.9238795325112867385, 1.000000000000000000, 0.9238795325112867385, 1.000000000000000000, 0.9238795325112867385, 1.000000000000000000, 0.9238795325112867385, 1.000000000000000000, 0.9238795325112867385, 1.000000000000000000, 0.9238795325112867385, 1.000000000000000000, 0.9238795325112867385, 1.000000000000000000, 0.9238795325112867385, 1.000000000000000000, 0.9238795325112867385, 1.000000000000000000, 0.9238795325112867385, 1.000000000000000000, 0.9238795325112867385, 1.000000000000000000, 0.9238795325112867385, 1.000000000000000000, 0.9238795325112867385, 1.000000000000000000, 0.9238795325112867385, 1.000000000000000000, 0.9238795325112867385, 1.000000000000000000, 0.9238795325112867385, 1.000000000000000000, 0.9238795325112867385, 1.000000000000000000, 0.9238795325112867385, 1.000000000000000000, 0.9238795325112867385, 1.000000000000000000, 0.9238795325112867385, 1.000000000000000000, 0.9238795325112867385, 1.000000000000000000, 0.9238795325112867385, 1.000000000000000000, 0.9238795325112867385, 1.000000000000000000, 0.9238795325112867385, 1.000000000000000000, 0.9238795325112867385, 1.000000000000000000, 0.9238795325112867385, 1.000000000000000000, 0.9238795325112867385, 1.000000000000000000, 0.9238795325112867385, 1.000000000000000000, 0.9238795325112867385, 1.000000000000000000, 0.9238795325112867385, 1.000000000000000000, 0.9238795325112867385, 1.000000000000000000, 0.9238795325112867385, 1.000000000000000000, 0.9238795325112867385, 1.000000000000000000, 0.9238795325112867385, 1.000000000000000000, 0.9238795325112867385, 1.000000000000000000, 0.9238795325112867385, 1.000000000000000000, 0.9238795325112867385, 1.000000000000000000, 0.9238795325112867385, 1.000000000000000000, 0.9238795325112867385, 1.000000000000000000, 0.9238795325112867385, 1.000000000000000000, 0.9238795325112867385, 1.000000000000000000, 0.9238795325112867385, 1.000000000000000000, 0.9238795325112867385, 1.000000000000000000, 0.9238795325112867385, 1.000000000000000000, 0.9238795325112867385, 1.000000000000000000, 0.9238795325112867385, 1.000000000000000000, 0.9238795325112867385, 1.000000000000000000, 0.9238795325112867385, 1.000000000000000000, 0.9238795325112867385, 1.000000000000000000, 0.9238795325112867385, 1.000000000000000000, 0.9238795325112867385, 1.000000000000000000, 0.9238795325112867385, 1.000000000000000000, 0.9238795325112867385, 1.000000000000000000, 0.9238795325112867385, 1.000000000000000000, 0.9238795325112867385, 1.000000000000000000, 0.9238795325112867385, 1.000000000000000000, 0.9238795325112867385, 1.000000000000000000, 0.9238795325112867385, 1.000000000000000000, 0.9238795325112867385, 1.000000000000000000, 0.9238795325112867385, 1.000000000000000000, 0.9238795325112867385, 1.000000000000000000) ) ) 
 REPRESENTATION_ITEM ( '' )  SURFACE ( )  );
#15248 = CARTESIAN_POINT ( 'NONE',  ( -25.62889119307865116, 0.2563525944202221796, -202.7491877320029801 ) ) ;
#15249 = AXIS2_PLACEMENT_3D ( 'NONE', #4577, #3487, #3407 ) ;
#15250 = CARTESIAN_POINT ( 'NONE',  ( 6.348887620881822791, 14.84416895885140875, 1.551339895120714685 ) ) ;
#15251 = CARTESIAN_POINT ( 'NONE',  ( -1.346194077712559167, 12.93750000000000178, -6.749999999999999112 ) ) ;
#15252 = PLANE ( 'NONE',  #2012 ) ;
#15253 = CARTESIAN_POINT ( 'NONE',  ( -3.750000000000000000, 0.6875000000000000000, -1.946699141100893149 ) ) ;
#15254 = FACE_OUTER_BOUND ( 'NONE', #1583, .T. ) ;
#15255 = CARTESIAN_POINT ( 'NONE',  ( -3.782526895735879524, 9.999999999999998224, -42.84475209785865246 ) ) ;
#15256 = CARTESIAN_POINT ( 'NONE',  ( 21.56941276937137530, 0.02712874445307413007, -138.7330449865694391 ) ) ;
#15257 = CARTESIAN_POINT ( 'NONE',  ( -5.856348882554203605, 2.099999999999253131, 27.66182687845087429 ) ) ;
#15258 = CARTESIAN_POINT ( 'NONE',  ( 3.249999999999998668, 10.68750000000000000, -4.846194077712560500 ) ) ;
#15259 = CARTESIAN_POINT ( 'NONE',  ( 26.22222779830891781, 1.749999999999999778, 70.75745246403606359 ) ) ;
#15260 = CARTESIAN_POINT ( 'NONE',  ( 30.32986759126112730, 0.7500000000000000000, 43.04214087805580391 ) ) ;
#15261 = ORIENTED_EDGE ( 'NONE', *, *, #5538, .F. ) ;
#15262 = ORIENTED_EDGE ( 'NONE', *, *, #9125, .T. ) ;
#15263 = FACE_OUTER_BOUND ( 'NONE', #5660, .T. ) ;
#15264 = CARTESIAN_POINT ( 'NONE',  ( -2.651650429449553314, 4.375000000000000000, -6.151650429449552426 ) ) ;
#15265 = CARTESIAN_POINT ( 'NONE',  ( -3.750000000000000000, 3.812500000000000000, -5.053300858899105741 ) ) ;
#15266 = CARTESIAN_POINT ( 'NONE',  ( -65.53364736412717662, 10.00000000000000000, -205.7441351029432894 ) ) ;
#15267 = ORIENTED_EDGE ( 'NONE', *, *, #1256, .T. ) ;
#15268 = CARTESIAN_POINT ( 'NONE',  ( -2.298097038856278918, 14.37500000000000000, -5.798097038856277585 ) ) ;
#15269 = CARTESIAN_POINT ( 'NONE',  ( -1.313187589810638212, 5.000000000000000000, -105.6642581345501526 ) ) ;
#15270 = CARTESIAN_POINT ( 'NONE',  ( 4.962552820103347528, 8.673617379884034486E-16, -121.4286218404057678 ) ) ;
#15271 = EDGE_CURVE ( 'NONE', #40, #6618, #9068, .T. ) ;
#15272 = CARTESIAN_POINT ( 'NONE',  ( 0.000000000000000000, 0.000000000000000000, 0.000000000000000000 ) ) ;
#15273 = CARTESIAN_POINT ( 'NONE',  ( -3.249999999999999556, 2.312500000000000888, -4.846194077712557835 ) ) ;
#15274 = COORDINATED_UNIVERSAL_TIME_OFFSET ( 0, 0, .AHEAD. ) ;
#15275 = CARTESIAN_POINT ( 'NONE',  ( 30.32986759126112730, 1.750000000000000000, 43.04214087805580391 ) ) ;
#15276 = CARTESIAN_POINT ( 'NONE',  ( 19.51808381314846841, 5.000000000000000888, -131.6416685809227545 ) ) ;
#15277 = VERTEX_POINT ( 'NONE', #6612 ) ;
#15278 = DIRECTION ( 'NONE',  ( -0.5024920151648518685, 0.000000000000000000, -0.8645818496218656835 ) ) ;
#15279 = CARTESIAN_POINT ( 'NONE',  ( 0.000000000000000000, 10.00000000000000000, -0.2500000000000002220 ) ) ;
#15280 = ORIENTED_EDGE ( 'NONE', *, *, #3869, .T. ) ;
#15281 = ORIENTED_EDGE ( 'NONE', *, *, #12424, .F. ) ;
#15282 = LINE ( 'NONE', #1050, #348 ) ;
#15283 = CARTESIAN_POINT ( 'NONE',  ( 3.750000000000000000, 5.312500000000000000, -1.946699141100892705 ) ) ;
#15284 = CARTESIAN_POINT ( 'NONE',  ( -3.980102097228897738E-16, 8.000000000000000000, -6.749999999999999112 ) ) ;
#15285 = ORIENTED_EDGE ( 'NONE', *, *, #1468, .T. ) ;
#15286 = CARTESIAN_POINT ( 'NONE',  ( 6.124339417936002228, 10.65787600314544470, 5.248591459689508021 ) ) ;
#15287 = CARTESIAN_POINT ( 'NONE',  ( -1.346194077712559389, 1.062500000000000222, -0.2500000000000002220 ) ) ;
#15288 = CARTESIAN_POINT ( 'NONE',  ( -2.651650429449553314, 9.375000000000000000, -6.151650429449552426 ) ) ;
#15289 = CARTESIAN_POINT ( 'NONE',  ( -25.38784507181503614, 1.060216903838750113, -206.1915231985982757 ) ) ;
#15290 = CARTESIAN_POINT ( 'NONE',  ( -2.276491945804053785, -4.336808689942018525E-15, -122.8215887834235787 ) ) ;
#15291 = ADVANCED_FACE ( 'NONE', ( #11170 ), #11319, .T. ) ;
#15292 = CIRCLE ( 'NONE', #8608, 3.000000000000010214 ) ;
#15293 = CARTESIAN_POINT ( 'NONE',  ( -8.289881740238515206, -2.529993217055220178, -35.21986562831452261 ) ) ;
#15294 = PERSON_AND_ORGANIZATION_ROLE ( 'creator' ) ;
#15295 = ADVANCED_FACE ( 'NONE', ( #3997 ), #13655, .F. ) ;
#15296 = DIRECTION ( 'NONE',  ( 0.8538457527776451839, 0.000000000000000000, 0.5205261093005582040 ) ) ;
#15297 = ORIENTED_EDGE ( 'NONE', *, *, #7026, .F. ) ;
#15298 = CARTESIAN_POINT ( 'NONE',  ( 3.249999999999998224, 5.312500000000000000, -2.153805922287439945 ) ) ;
#15299 = CARTESIAN_POINT ( 'NONE',  ( -6.805338252203106286, 1.921202954650395478, -45.13192727926512759 ) ) ;
#15300 = CARTESIAN_POINT ( 'NONE',  ( -1.553300858899106629, 12.56250000000000355, 0.2499999999999998335 ) ) ;
#15301 = CARTESIAN_POINT ( 'NONE',  ( 1.049898006922821869, 4.588323854676484181, -139.4675471490223515 ) ) ;
#15302 = CARTESIAN_POINT ( 'NONE',  ( -66.08772900935203154, 15.00301221266680862, -199.0286653353512634 ) ) ;
#15303 = CARTESIAN_POINT ( 'NONE',  ( -1.286431735982999758, 5.000000000000007105, -134.7299422376718496 ) ) ;
#15304 = CARTESIAN_POINT ( 'NONE',  ( -1.346194077712558945, 0.5625000000000003331, -0.2500000000000002220 ) ) ;
#15305 = CARTESIAN_POINT ( 'NONE',  ( -3.184492023421114926, 4.336808689942017736E-16, -109.5142639673473468 ) ) ;
#15306 = EDGE_CURVE ( 'NONE', #1079, #13758, #4978, .T. ) ;
#15307 = PERSON_AND_ORGANIZATION_ROLE ( 'classification_officer' ) ;
#15308 = CARTESIAN_POINT ( 'NONE',  ( -2.298097038856278473, 14.12500000000000000, -1.201902961143720416 ) ) ;
#15309 = CIRCLE ( 'NONE', #5665, 2.250000000000005773 ) ;
#15310 = CARTESIAN_POINT ( 'NONE',  ( -1.376260179405567108, 15.00000000000000000, -106.6458321843530683 ) ) ;
#15311 = AXIS2_PLACEMENT_3D ( 'NONE', #948, #3340, #12698 ) ;
#15312 = VERTEX_POINT ( 'NONE', #7538 ) ;
#15313 = CARTESIAN_POINT ( 'NONE',  ( -25.80176686614077042, -6.001942919173320219E-12, -207.3616737857323642 ) ) ;
#15314 = CARTESIAN_POINT ( 'NONE',  ( -3.249999999999999556, 2.312500000000000888, -4.846194077712557835 ) ) ;
#15315 = CARTESIAN_POINT ( 'NONE',  ( -6.965072737286399196, 4.013953217152291696E-15, -104.2966754940355827 ) ) ;
#15316 = VECTOR ( 'NONE', #8711, 1000.000000000000000 ) ;
#15317 = NEXT_ASSEMBLY_USAGE_OCCURRENCE ( 'NAUO1', ' ', ' ', #10001, #2439, $ ) ;
#15318 = NEXT_ASSEMBLY_USAGE_OCCURRENCE ( 'NAUO2', ' ', ' ', #10001, #8846, $ ) ;
#15319 = NEXT_ASSEMBLY_USAGE_OCCURRENCE ( 'NAUO3', ' ', ' ', #10001, #10487, $ ) ;
#15320 = NEXT_ASSEMBLY_USAGE_OCCURRENCE ( 'NAUO4', ' ', ' ', #10001, #8872, $ ) ;
#15321 = NEXT_ASSEMBLY_USAGE_OCCURRENCE ( 'NAUO5', ' ', ' ', #10001, #8454, $ ) ;
#15322 = NEXT_ASSEMBLY_USAGE_OCCURRENCE ( 'NAUO6', ' ', ' ', #10001, #2984, $ ) ;
#15323 = NEXT_ASSEMBLY_USAGE_OCCURRENCE ( 'NAUO7', ' ', ' ', #10001, #1046, $ ) ;
#15324 = NEXT_ASSEMBLY_USAGE_OCCURRENCE ( 'NAUO8', ' ', ' ', #10001, #9258, $ ) ;
#15325 = COLOUR_RGB('Deep Blue', 0.66274510, 0.83137255, 0.94901961);
#15326 = FILL_AREA_STYLE_COLOUR('',#15325);
#15327 = FILL_AREA_STYLE('',(#15326));
#15328 = SURFACE_STYLE_FILL_AREA(#15327);
#15329 = SURFACE_SIDE_STYLE('',(#15328));
#15330 = SURFACE_STYLE_USAGE(.BOTH.,#15329);
#15331 = PRESENTATION_STYLE_ASSIGNMENT((#15330));
#15332 = COLOUR_RGB('Light Blue', 0.31764706, 0.68627451, 0.89019608);
#15333 = FILL_AREA_STYLE_COLOUR('',#15332);
#15334 = FILL_AREA_STYLE('',(#15333));
#15335 = SURFACE_STYLE_FILL_AREA(#15334);
#15336 = SURFACE_SIDE_STYLE('',(#15335));
#15337 = SURFACE_STYLE_USAGE(.BOTH.,#15336);
#15338 = PRESENTATION_STYLE_ASSIGNMENT((#15337));
#15339 = COLOUR_RGB('Sky Blue', 0.40784314, 0.44705882, 0.49803922);
#15340 = FILL_AREA_STYLE_COLOUR('',#15339);
#15341 = FILL_AREA_STYLE('',(#15340));
#15342 = SURFACE_STYLE_FILL_AREA(#15341);
#15343 = SURFACE_SIDE_STYLE('',(#15342));
#15344 = SURFACE_STYLE_USAGE(.BOTH.,#15343);
#15345 = PRESENTATION_STYLE_ASSIGNMENT((#15344));
#15346 = COLOUR_RGB('Slate Gray', 0.72549020, 0.75294118, 0.79215686);
#15347 = FILL_AREA_STYLE_COLOUR('',#15346);
#15348 = FILL_AREA_STYLE('',(#15347));
#15349 = SURFACE_STYLE_FILL_AREA(#15348);
#15350 = SURFACE_SIDE_STYLE('',(#15349));
#15351 = SURFACE_STYLE_USAGE(.BOTH.,#15350);
#15352 = PRESENTATION_STYLE_ASSIGNMENT((#15351));
#15353 = COLOUR_RGB('Light Gray', 0.08235294, 0.09019608, 0.10196078);
#15354 = FILL_AREA_STYLE_COLOUR('',#15353);
#15355 = FILL_AREA_STYLE('',(#15354));
#15356 = SURFACE_STYLE_FILL_AREA(#15355);
#15357 = SURFACE_SIDE_STYLE('',(#15356));
#15358 = SURFACE_STYLE_USAGE(.BOTH.,#15357);
#15359 = PRESENTATION_STYLE_ASSIGNMENT((#15358));
#15360 = COLOUR_RGB('Black', 0.09019608, 0.27058824, 0.51372549);
#15361 = FILL_AREA_STYLE_COLOUR('',#15360);
#15362 = FILL_AREA_STYLE('',(#15361));
#15363 = SURFACE_STYLE_FILL_AREA(#15362);
#15364 = SURFACE_SIDE_STYLE('',(#15363));
#15365 = SURFACE_STYLE_USAGE(.BOTH.,#15364);
#15366 = PRESENTATION_STYLE_ASSIGNMENT((#15365));
#15367 = STYLED_ITEM('',(#15345),#7115);
#15368 = MECHANICAL_DESIGN_GEOMETRIC_PRESENTATION_REPRESENTATION('',(#15367),#6710);
#15369 = STYLED_ITEM('',(#15359),#7543);
#15370 = MECHANICAL_DESIGN_GEOMETRIC_PRESENTATION_REPRESENTATION('',(#15369),#2511);
#15371 = STYLED_ITEM('',(#15338),#12454);
#15372 = MECHANICAL_DESIGN_GEOMETRIC_PRESENTATION_REPRESENTATION('',(#15371),#12893);
#15373 = STYLED_ITEM('',(#15338),#2311);
#15374 = MECHANICAL_DESIGN_GEOMETRIC_PRESENTATION_REPRESENTATION('',(#15373),#14368);
#15375 = STYLED_ITEM('',(#15366),#12143);
#15376 = MECHANICAL_DESIGN_GEOMETRIC_PRESENTATION_REPRESENTATION('',(#15375),#1768);
#15377 = STYLED_ITEM('',(#15331),#2140);
#15378 = MECHANICAL_DESIGN_GEOMETRIC_PRESENTATION_REPRESENTATION('',(#15377),#3238);
#15379 = STYLED_ITEM('',(#15331),#12195);
#15380 = MECHANICAL_DESIGN_GEOMETRIC_PRESENTATION_REPRESENTATION('',(#15379),#11867);
#15381 = STYLED_ITEM('',(#15352),#7440);
#15382 = MECHANICAL_DESIGN_GEOMETRIC_PRESENTATION_REPRESENTATION('',(#15381),#6228);
ENDSEC;
END-ISO-10303-21;
